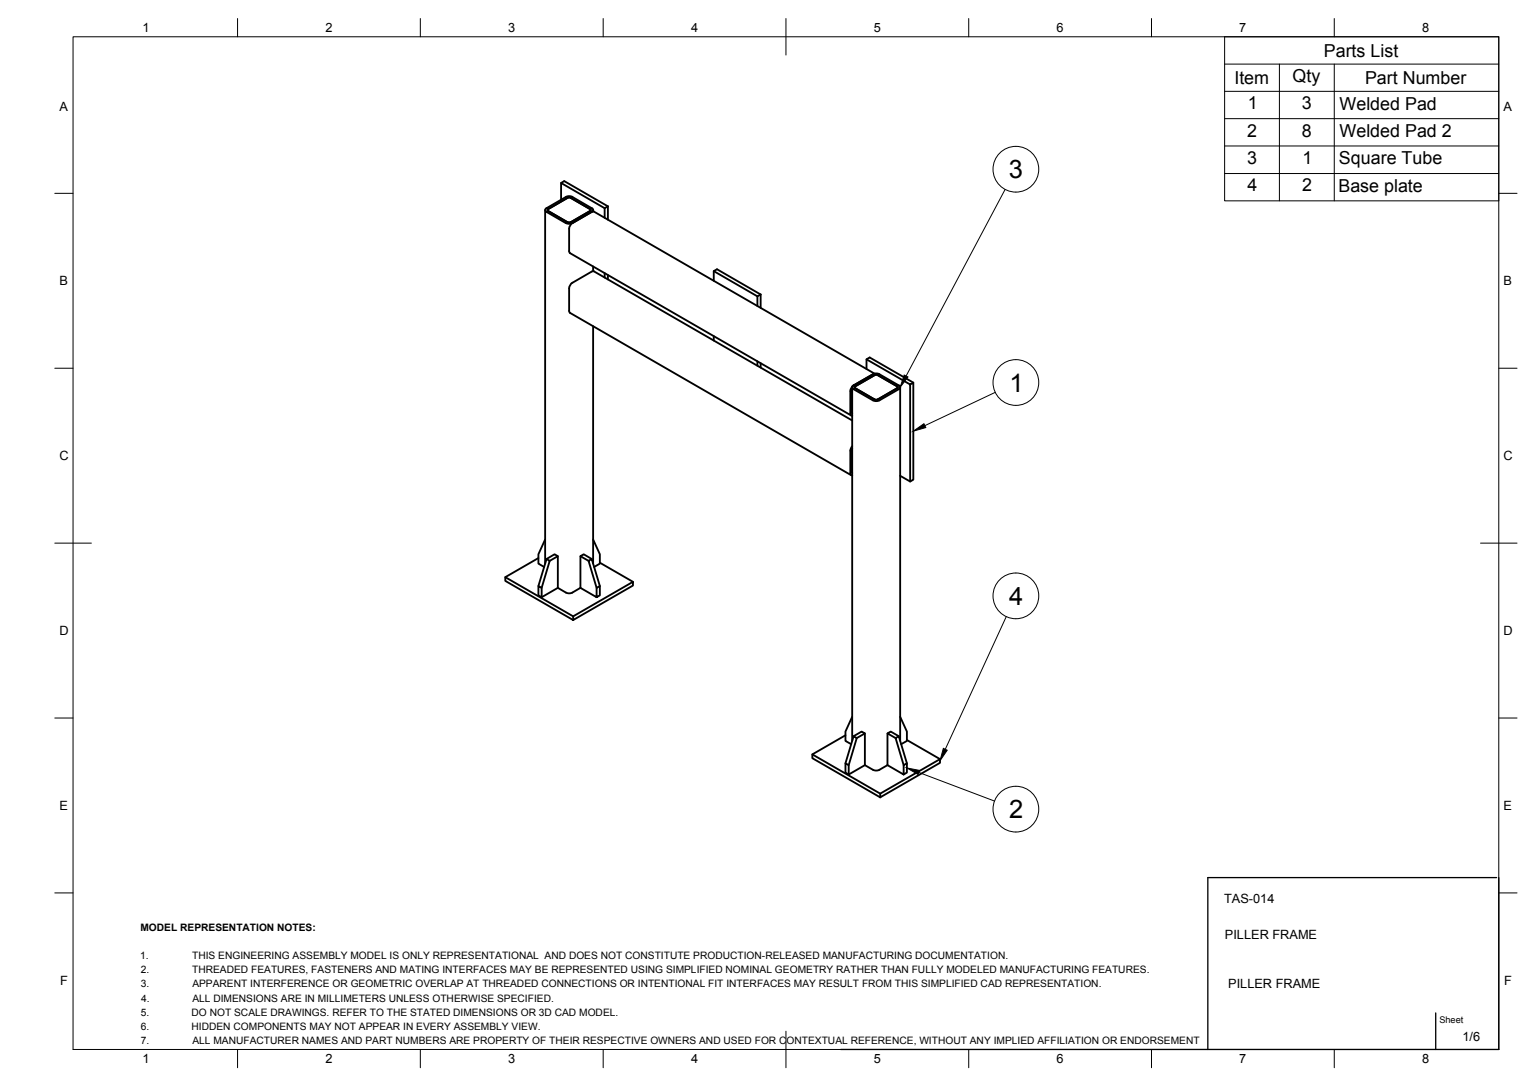
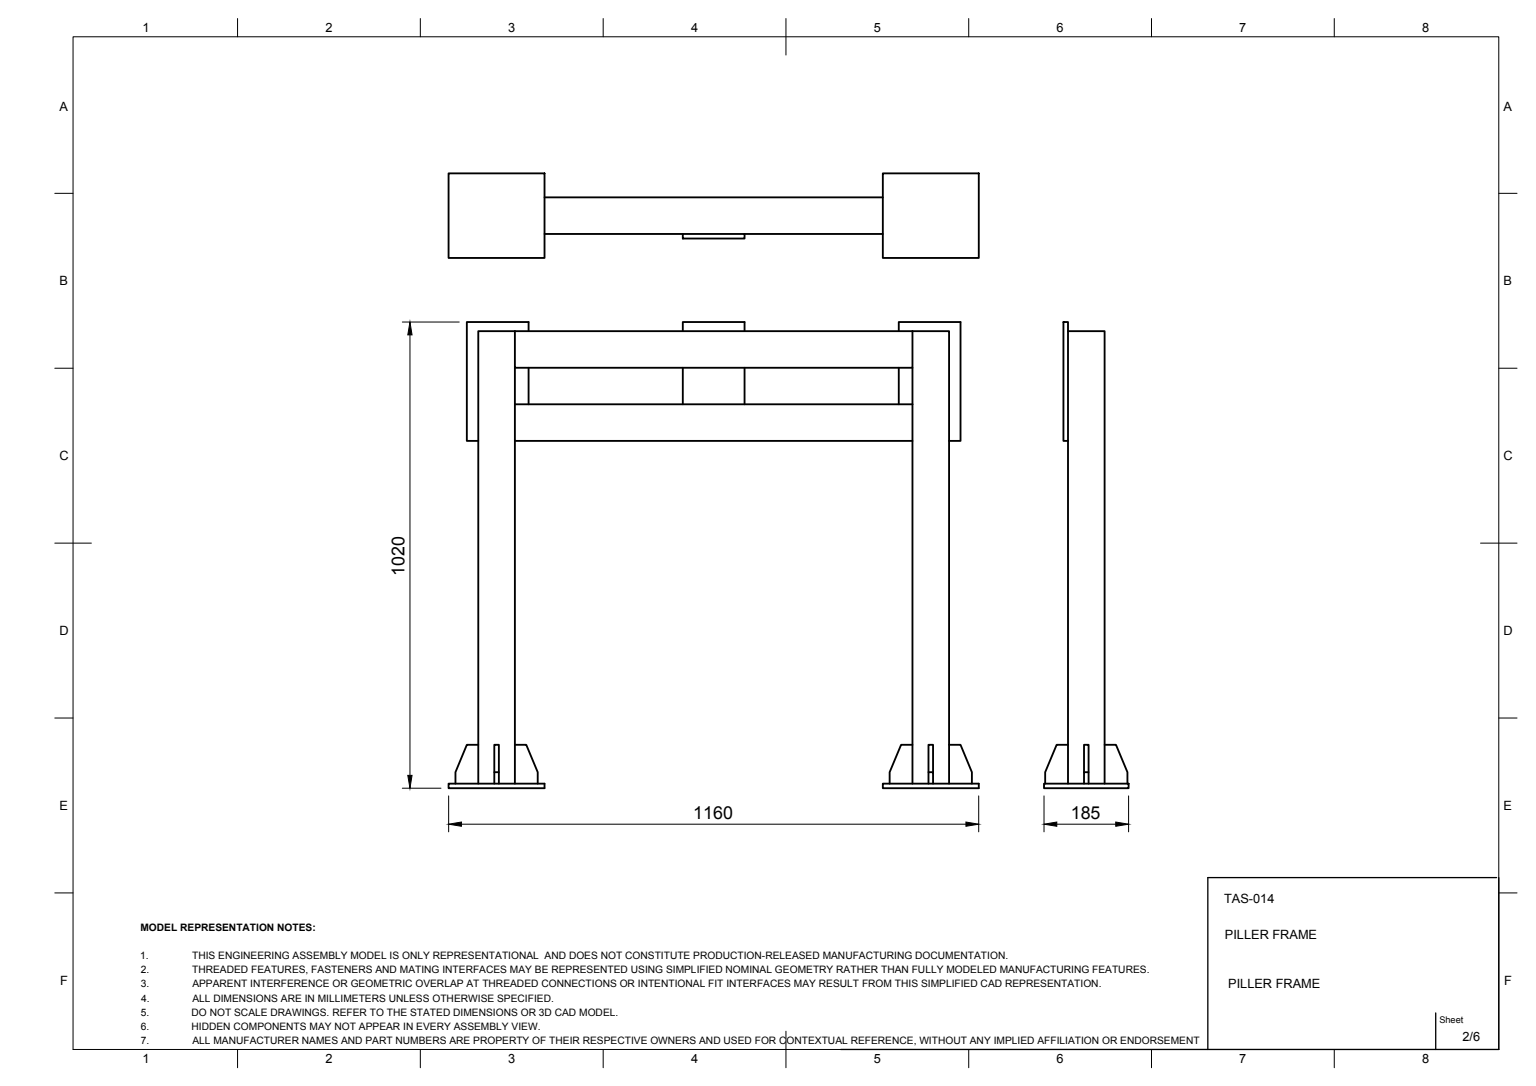
ISO-10303-21;
HEADER;
/* Generated by software containing ST-Developer
 * from STEP Tools, Inc. (www.steptools.com) 
 */

FILE_DESCRIPTION(
/* description */ ('STEP AP214'),
/* implementation_level */ '2;1');

FILE_NAME(
/* name */ 'TAS-014.step',
/* time_stamp */ '2026-11-15T15:22:30-08:00',
/* author */ (''),
/* organization */ (''),
/* preprocessor_version */ 'ST-DEVELOPER v20.2',
/* originating_system */ 'Autodesk Translation Framework v15.17.0.0',
/* authorisation */ '');

FILE_SCHEMA (('AUTOMOTIVE_DESIGN { 1 0 10303 214 3 1 1 }'));
ENDSEC;

DATA;
#10=MECHANICAL_DESIGN_GEOMETRIC_PRESENTATION_REPRESENTATION('',(#79,#80,
#81,#82,#83,#84,#85,#86,#87),#3119);
#11=ITEM_DEFINED_TRANSFORMATION($,$,#2000,#2022);
#12=ITEM_DEFINED_TRANSFORMATION($,$,#2014,#2023);
#13=ITEM_DEFINED_TRANSFORMATION($,$,#1853,#2024);
#14=ITEM_DEFINED_TRANSFORMATION($,$,#2007,#2025);
#15=ITEM_DEFINED_TRANSFORMATION($,$,#2000,#2026);
#16=ITEM_DEFINED_TRANSFORMATION($,$,#2014,#2027);
#17=ITEM_DEFINED_TRANSFORMATION($,$,#2014,#2028);
#18=ITEM_DEFINED_TRANSFORMATION($,$,#2014,#2029);
#19=ITEM_DEFINED_TRANSFORMATION($,$,#2000,#2030);
#20=ITEM_DEFINED_TRANSFORMATION($,$,#2007,#2031);
#21=ITEM_DEFINED_TRANSFORMATION($,$,#2014,#2032);
#22=ITEM_DEFINED_TRANSFORMATION($,$,#2014,#2033);
#23=ITEM_DEFINED_TRANSFORMATION($,$,#2014,#2034);
#24=ITEM_DEFINED_TRANSFORMATION($,$,#2014,#2035);
#25=(
REPRESENTATION_RELATIONSHIP($,$,#3150,#3148)
REPRESENTATION_RELATIONSHIP_WITH_TRANSFORMATION(#11)
SHAPE_REPRESENTATION_RELATIONSHIP()
);
#26=(
REPRESENTATION_RELATIONSHIP($,$,#3152,#3148)
REPRESENTATION_RELATIONSHIP_WITH_TRANSFORMATION(#12)
SHAPE_REPRESENTATION_RELATIONSHIP()
);
#27=(
REPRESENTATION_RELATIONSHIP($,$,#3149,#3148)
REPRESENTATION_RELATIONSHIP_WITH_TRANSFORMATION(#13)
SHAPE_REPRESENTATION_RELATIONSHIP()
);
#28=(
REPRESENTATION_RELATIONSHIP($,$,#3151,#3148)
REPRESENTATION_RELATIONSHIP_WITH_TRANSFORMATION(#14)
SHAPE_REPRESENTATION_RELATIONSHIP()
);
#29=(
REPRESENTATION_RELATIONSHIP($,$,#3150,#3148)
REPRESENTATION_RELATIONSHIP_WITH_TRANSFORMATION(#15)
SHAPE_REPRESENTATION_RELATIONSHIP()
);
#30=(
REPRESENTATION_RELATIONSHIP($,$,#3152,#3148)
REPRESENTATION_RELATIONSHIP_WITH_TRANSFORMATION(#16)
SHAPE_REPRESENTATION_RELATIONSHIP()
);
#31=(
REPRESENTATION_RELATIONSHIP($,$,#3152,#3148)
REPRESENTATION_RELATIONSHIP_WITH_TRANSFORMATION(#17)
SHAPE_REPRESENTATION_RELATIONSHIP()
);
#32=(
REPRESENTATION_RELATIONSHIP($,$,#3152,#3148)
REPRESENTATION_RELATIONSHIP_WITH_TRANSFORMATION(#18)
SHAPE_REPRESENTATION_RELATIONSHIP()
);
#33=(
REPRESENTATION_RELATIONSHIP($,$,#3150,#3148)
REPRESENTATION_RELATIONSHIP_WITH_TRANSFORMATION(#19)
SHAPE_REPRESENTATION_RELATIONSHIP()
);
#34=(
REPRESENTATION_RELATIONSHIP($,$,#3151,#3148)
REPRESENTATION_RELATIONSHIP_WITH_TRANSFORMATION(#20)
SHAPE_REPRESENTATION_RELATIONSHIP()
);
#35=(
REPRESENTATION_RELATIONSHIP($,$,#3152,#3148)
REPRESENTATION_RELATIONSHIP_WITH_TRANSFORMATION(#21)
SHAPE_REPRESENTATION_RELATIONSHIP()
);
#36=(
REPRESENTATION_RELATIONSHIP($,$,#3152,#3148)
REPRESENTATION_RELATIONSHIP_WITH_TRANSFORMATION(#22)
SHAPE_REPRESENTATION_RELATIONSHIP()
);
#37=(
REPRESENTATION_RELATIONSHIP($,$,#3152,#3148)
REPRESENTATION_RELATIONSHIP_WITH_TRANSFORMATION(#23)
SHAPE_REPRESENTATION_RELATIONSHIP()
);
#38=(
REPRESENTATION_RELATIONSHIP($,$,#3152,#3148)
REPRESENTATION_RELATIONSHIP_WITH_TRANSFORMATION(#24)
SHAPE_REPRESENTATION_RELATIONSHIP()
);
#39=CONTEXT_DEPENDENT_SHAPE_REPRESENTATION(#25,#3134);
#40=CONTEXT_DEPENDENT_SHAPE_REPRESENTATION(#26,#3135);
#41=CONTEXT_DEPENDENT_SHAPE_REPRESENTATION(#27,#3136);
#42=CONTEXT_DEPENDENT_SHAPE_REPRESENTATION(#28,#3137);
#43=CONTEXT_DEPENDENT_SHAPE_REPRESENTATION(#29,#3138);
#44=CONTEXT_DEPENDENT_SHAPE_REPRESENTATION(#30,#3139);
#45=CONTEXT_DEPENDENT_SHAPE_REPRESENTATION(#31,#3140);
#46=CONTEXT_DEPENDENT_SHAPE_REPRESENTATION(#32,#3141);
#47=CONTEXT_DEPENDENT_SHAPE_REPRESENTATION(#33,#3142);
#48=CONTEXT_DEPENDENT_SHAPE_REPRESENTATION(#34,#3143);
#49=CONTEXT_DEPENDENT_SHAPE_REPRESENTATION(#35,#3144);
#50=CONTEXT_DEPENDENT_SHAPE_REPRESENTATION(#36,#3145);
#51=CONTEXT_DEPENDENT_SHAPE_REPRESENTATION(#37,#3146);
#52=CONTEXT_DEPENDENT_SHAPE_REPRESENTATION(#38,#3147);
#53=NEXT_ASSEMBLY_USAGE_OCCURRENCE('Welded Pad:1','Welded Pad:1',
'Welded Pad:1',#3154,#3156,'Welded Pad:1');
#54=NEXT_ASSEMBLY_USAGE_OCCURRENCE('Welded Pad 2:1','Welded Pad 2:1',
'Welded Pad 2:1',#3154,#3158,'Welded Pad 2:1');
#55=NEXT_ASSEMBLY_USAGE_OCCURRENCE('Square Tube:1','Square Tube:1',
'Square Tube:1',#3154,#3155,'Square Tube:1');
#56=NEXT_ASSEMBLY_USAGE_OCCURRENCE('Base Plate:1','Base Plate:1',
'Base Plate:1',#3154,#3157,'Base Plate:1');
#57=NEXT_ASSEMBLY_USAGE_OCCURRENCE('Welded Pad:2','Welded Pad:2',
'Welded Pad:2',#3154,#3156,'Welded Pad:2');
#58=NEXT_ASSEMBLY_USAGE_OCCURRENCE('Welded Pad 2:2','Welded Pad 2:2',
'Welded Pad 2:2',#3154,#3158,'Welded Pad 2:2');
#59=NEXT_ASSEMBLY_USAGE_OCCURRENCE('Welded Pad 2:3','Welded Pad 2:3',
'Welded Pad 2:3',#3154,#3158,'Welded Pad 2:3');
#60=NEXT_ASSEMBLY_USAGE_OCCURRENCE('Welded Pad 2:4','Welded Pad 2:4',
'Welded Pad 2:4',#3154,#3158,'Welded Pad 2:4');
#61=NEXT_ASSEMBLY_USAGE_OCCURRENCE('Welded Pad:3','Welded Pad:3',
'Welded Pad:3',#3154,#3156,'Welded Pad:3');
#62=NEXT_ASSEMBLY_USAGE_OCCURRENCE('Base Plate:2','Base Plate:2',
'Base Plate:2',#3154,#3157,'Base Plate:2');
#63=NEXT_ASSEMBLY_USAGE_OCCURRENCE('Welded Pad 2:5','Welded Pad 2:5',
'Welded Pad 2:5',#3154,#3158,'Welded Pad 2:5');
#64=NEXT_ASSEMBLY_USAGE_OCCURRENCE('Welded Pad 2:6','Welded Pad 2:6',
'Welded Pad 2:6',#3154,#3158,'Welded Pad 2:6');
#65=NEXT_ASSEMBLY_USAGE_OCCURRENCE('Welded Pad 2:7','Welded Pad 2:7',
'Welded Pad 2:7',#3154,#3158,'Welded Pad 2:7');
#66=NEXT_ASSEMBLY_USAGE_OCCURRENCE('Welded Pad 2:8','Welded Pad 2:8',
'Welded Pad 2:8',#3154,#3158,'Welded Pad 2:8');
#67=SHAPE_REPRESENTATION_RELATIONSHIP('SRR','None',#3149,#71);
#68=SHAPE_REPRESENTATION_RELATIONSHIP('SRR','None',#3150,#72);
#69=SHAPE_REPRESENTATION_RELATIONSHIP('SRR','None',#3151,#73);
#70=SHAPE_REPRESENTATION_RELATIONSHIP('SRR','None',#3152,#74);
#71=ADVANCED_BREP_SHAPE_REPRESENTATION('',(#88,#89,#90,#91),#3115);
#72=ADVANCED_BREP_SHAPE_REPRESENTATION('',(#92),#3116);
#73=ADVANCED_BREP_SHAPE_REPRESENTATION('',(#93),#3117);
#74=ADVANCED_BREP_SHAPE_REPRESENTATION('',(#94),#3118);
#75=OPEN_SHELL('',(#1779));
#76=OPEN_SHELL('',(#1780));
#77=SHELL_BASED_SURFACE_MODEL('Body5',(#75));
#78=SHELL_BASED_SURFACE_MODEL('Body6',(#76));
#79=STYLED_ITEM('',(#3178),#88);
#80=STYLED_ITEM('',(#3178),#89);
#81=STYLED_ITEM('',(#3178),#90);
#82=STYLED_ITEM('',(#3178),#91);
#83=STYLED_ITEM('',(#3178),#77);
#84=STYLED_ITEM('',(#3178),#78);
#85=STYLED_ITEM('',(#3178),#92);
#86=STYLED_ITEM('',(#3178),#93);
#87=STYLED_ITEM('',(#3178),#94);
#88=MANIFOLD_SOLID_BREP('Body1',#1800);
#89=MANIFOLD_SOLID_BREP('Body2',#1801);
#90=MANIFOLD_SOLID_BREP('Body3',#1802);
#91=MANIFOLD_SOLID_BREP('Body4',#1803);
#92=MANIFOLD_SOLID_BREP('Body1',#1804);
#93=MANIFOLD_SOLID_BREP('Body1',#1805);
#94=MANIFOLD_SOLID_BREP('Body1',#1806);
#95=FACE_BOUND('',#317,.T.);
#96=FACE_BOUND('',#319,.T.);
#97=FACE_BOUND('',#337,.T.);
#98=FACE_BOUND('',#339,.T.);
#99=FACE_BOUND('',#357,.T.);
#100=FACE_BOUND('',#359,.T.);
#101=FACE_BOUND('',#377,.T.);
#102=FACE_BOUND('',#379,.T.);
#103=CIRCLE('',#1856,5.);
#104=CIRCLE('',#1857,5.);
#105=CIRCLE('',#1860,5.);
#106=CIRCLE('',#1861,5.);
#107=CIRCLE('',#1864,5.);
#108=CIRCLE('',#1865,5.);
#109=CIRCLE('',#1868,5.);
#110=CIRCLE('',#1869,5.);
#111=CIRCLE('',#1872,10.);
#112=CIRCLE('',#1873,10.);
#113=CIRCLE('',#1876,10.);
#114=CIRCLE('',#1877,10.);
#115=CIRCLE('',#1880,10.);
#116=CIRCLE('',#1881,10.);
#117=CIRCLE('',#1884,10.);
#118=CIRCLE('',#1885,10.);
#119=CIRCLE('',#1890,5.);
#120=CIRCLE('',#1891,5.);
#121=CIRCLE('',#1894,5.);
#122=CIRCLE('',#1895,5.);
#123=CIRCLE('',#1898,5.);
#124=CIRCLE('',#1899,5.);
#125=CIRCLE('',#1902,5.);
#126=CIRCLE('',#1903,5.);
#127=CIRCLE('',#1906,10.);
#128=CIRCLE('',#1907,10.);
#129=CIRCLE('',#1910,10.);
#130=CIRCLE('',#1911,10.);
#131=CIRCLE('',#1914,10.);
#132=CIRCLE('',#1915,10.);
#133=CIRCLE('',#1918,10.);
#134=CIRCLE('',#1919,10.);
#135=CIRCLE('',#1923,10.);
#136=CIRCLE('',#1924,10.);
#137=CIRCLE('',#1927,10.);
#138=CIRCLE('',#1928,10.);
#139=CIRCLE('',#1931,10.);
#140=CIRCLE('',#1932,10.);
#141=CIRCLE('',#1935,10.);
#142=CIRCLE('',#1936,10.);
#143=CIRCLE('',#1938,5.);
#144=CIRCLE('',#1939,5.);
#145=CIRCLE('',#1942,5.);
#146=CIRCLE('',#1943,5.);
#147=CIRCLE('',#1946,5.);
#148=CIRCLE('',#1947,5.);
#149=CIRCLE('',#1950,5.);
#150=CIRCLE('',#1951,5.);
#151=CIRCLE('',#1957,10.);
#152=CIRCLE('',#1958,10.);
#153=CIRCLE('',#1961,10.);
#154=CIRCLE('',#1962,10.);
#155=CIRCLE('',#1965,10.);
#156=CIRCLE('',#1966,10.);
#157=CIRCLE('',#1969,10.);
#158=CIRCLE('',#1970,10.);
#159=CIRCLE('',#1972,5.);
#160=CIRCLE('',#1973,5.);
#161=CIRCLE('',#1976,5.);
#162=CIRCLE('',#1977,5.);
#163=CIRCLE('',#1980,5.);
#164=CIRCLE('',#1981,5.);
#165=CIRCLE('',#1984,5.);
#166=CIRCLE('',#1985,5.);
#167=CIRCLE('',#1991,5.);
#168=CIRCLE('',#1992,5.);
#169=CIRCLE('',#1993,5.);
#170=CIRCLE('',#1994,5.);
#171=CIRCLE('',#1996,5.);
#172=CIRCLE('',#1997,5.);
#173=CIRCLE('',#1998,5.);
#174=CIRCLE('',#1999,5.);
#175=CYLINDRICAL_SURFACE('',#1855,5.);
#176=CYLINDRICAL_SURFACE('',#1859,5.);
#177=CYLINDRICAL_SURFACE('',#1863,5.);
#178=CYLINDRICAL_SURFACE('',#1867,5.);
#179=CYLINDRICAL_SURFACE('',#1871,10.);
#180=CYLINDRICAL_SURFACE('',#1875,10.);
#181=CYLINDRICAL_SURFACE('',#1879,10.);
#182=CYLINDRICAL_SURFACE('',#1883,10.);
#183=CYLINDRICAL_SURFACE('',#1889,5.);
#184=CYLINDRICAL_SURFACE('',#1893,5.);
#185=CYLINDRICAL_SURFACE('',#1897,5.);
#186=CYLINDRICAL_SURFACE('',#1901,5.);
#187=CYLINDRICAL_SURFACE('',#1905,10.);
#188=CYLINDRICAL_SURFACE('',#1909,10.);
#189=CYLINDRICAL_SURFACE('',#1913,10.);
#190=CYLINDRICAL_SURFACE('',#1917,10.);
#191=CYLINDRICAL_SURFACE('',#1922,10.);
#192=CYLINDRICAL_SURFACE('',#1926,10.);
#193=CYLINDRICAL_SURFACE('',#1930,10.);
#194=CYLINDRICAL_SURFACE('',#1934,10.);
#195=CYLINDRICAL_SURFACE('',#1937,5.);
#196=CYLINDRICAL_SURFACE('',#1941,5.);
#197=CYLINDRICAL_SURFACE('',#1945,5.);
#198=CYLINDRICAL_SURFACE('',#1949,5.);
#199=CYLINDRICAL_SURFACE('',#1956,10.);
#200=CYLINDRICAL_SURFACE('',#1960,10.);
#201=CYLINDRICAL_SURFACE('',#1964,10.);
#202=CYLINDRICAL_SURFACE('',#1968,10.);
#203=CYLINDRICAL_SURFACE('',#1971,5.);
#204=CYLINDRICAL_SURFACE('',#1975,5.);
#205=CYLINDRICAL_SURFACE('',#1979,5.);
#206=CYLINDRICAL_SURFACE('',#1983,5.);
#207=FACE_OUTER_BOUND('',#300,.T.);
#208=FACE_OUTER_BOUND('',#301,.T.);
#209=FACE_OUTER_BOUND('',#302,.T.);
#210=FACE_OUTER_BOUND('',#303,.T.);
#211=FACE_OUTER_BOUND('',#304,.T.);
#212=FACE_OUTER_BOUND('',#305,.T.);
#213=FACE_OUTER_BOUND('',#306,.T.);
#214=FACE_OUTER_BOUND('',#307,.T.);
#215=FACE_OUTER_BOUND('',#308,.T.);
#216=FACE_OUTER_BOUND('',#309,.T.);
#217=FACE_OUTER_BOUND('',#310,.T.);
#218=FACE_OUTER_BOUND('',#311,.T.);
#219=FACE_OUTER_BOUND('',#312,.T.);
#220=FACE_OUTER_BOUND('',#313,.T.);
#221=FACE_OUTER_BOUND('',#314,.T.);
#222=FACE_OUTER_BOUND('',#315,.T.);
#223=FACE_OUTER_BOUND('',#316,.T.);
#224=FACE_OUTER_BOUND('',#318,.T.);
#225=FACE_OUTER_BOUND('',#320,.T.);
#226=FACE_OUTER_BOUND('',#321,.T.);
#227=FACE_OUTER_BOUND('',#322,.T.);
#228=FACE_OUTER_BOUND('',#323,.T.);
#229=FACE_OUTER_BOUND('',#324,.T.);
#230=FACE_OUTER_BOUND('',#325,.T.);
#231=FACE_OUTER_BOUND('',#326,.T.);
#232=FACE_OUTER_BOUND('',#327,.T.);
#233=FACE_OUTER_BOUND('',#328,.T.);
#234=FACE_OUTER_BOUND('',#329,.T.);
#235=FACE_OUTER_BOUND('',#330,.T.);
#236=FACE_OUTER_BOUND('',#331,.T.);
#237=FACE_OUTER_BOUND('',#332,.T.);
#238=FACE_OUTER_BOUND('',#333,.T.);
#239=FACE_OUTER_BOUND('',#334,.T.);
#240=FACE_OUTER_BOUND('',#335,.T.);
#241=FACE_OUTER_BOUND('',#336,.T.);
#242=FACE_OUTER_BOUND('',#338,.T.);
#243=FACE_OUTER_BOUND('',#340,.T.);
#244=FACE_OUTER_BOUND('',#341,.T.);
#245=FACE_OUTER_BOUND('',#342,.T.);
#246=FACE_OUTER_BOUND('',#343,.T.);
#247=FACE_OUTER_BOUND('',#344,.T.);
#248=FACE_OUTER_BOUND('',#345,.T.);
#249=FACE_OUTER_BOUND('',#346,.T.);
#250=FACE_OUTER_BOUND('',#347,.T.);
#251=FACE_OUTER_BOUND('',#348,.T.);
#252=FACE_OUTER_BOUND('',#349,.T.);
#253=FACE_OUTER_BOUND('',#350,.T.);
#254=FACE_OUTER_BOUND('',#351,.T.);
#255=FACE_OUTER_BOUND('',#352,.T.);
#256=FACE_OUTER_BOUND('',#353,.T.);
#257=FACE_OUTER_BOUND('',#354,.T.);
#258=FACE_OUTER_BOUND('',#355,.T.);
#259=FACE_OUTER_BOUND('',#356,.T.);
#260=FACE_OUTER_BOUND('',#358,.T.);
#261=FACE_OUTER_BOUND('',#360,.T.);
#262=FACE_OUTER_BOUND('',#361,.T.);
#263=FACE_OUTER_BOUND('',#362,.T.);
#264=FACE_OUTER_BOUND('',#363,.T.);
#265=FACE_OUTER_BOUND('',#364,.T.);
#266=FACE_OUTER_BOUND('',#365,.T.);
#267=FACE_OUTER_BOUND('',#366,.T.);
#268=FACE_OUTER_BOUND('',#367,.T.);
#269=FACE_OUTER_BOUND('',#368,.T.);
#270=FACE_OUTER_BOUND('',#369,.T.);
#271=FACE_OUTER_BOUND('',#370,.T.);
#272=FACE_OUTER_BOUND('',#371,.T.);
#273=FACE_OUTER_BOUND('',#372,.T.);
#274=FACE_OUTER_BOUND('',#373,.T.);
#275=FACE_OUTER_BOUND('',#374,.T.);
#276=FACE_OUTER_BOUND('',#375,.T.);
#277=FACE_OUTER_BOUND('',#376,.T.);
#278=FACE_OUTER_BOUND('',#378,.T.);
#279=FACE_OUTER_BOUND('',#380,.T.);
#280=FACE_OUTER_BOUND('',#381,.T.);
#281=FACE_OUTER_BOUND('',#382,.T.);
#282=FACE_OUTER_BOUND('',#383,.T.);
#283=FACE_OUTER_BOUND('',#384,.T.);
#284=FACE_OUTER_BOUND('',#385,.T.);
#285=FACE_OUTER_BOUND('',#386,.T.);
#286=FACE_OUTER_BOUND('',#387,.T.);
#287=FACE_OUTER_BOUND('',#388,.T.);
#288=FACE_OUTER_BOUND('',#389,.T.);
#289=FACE_OUTER_BOUND('',#390,.T.);
#290=FACE_OUTER_BOUND('',#391,.T.);
#291=FACE_OUTER_BOUND('',#392,.T.);
#292=FACE_OUTER_BOUND('',#393,.T.);
#293=FACE_OUTER_BOUND('',#394,.T.);
#294=FACE_OUTER_BOUND('',#395,.T.);
#295=FACE_OUTER_BOUND('',#396,.T.);
#296=FACE_OUTER_BOUND('',#397,.T.);
#297=FACE_OUTER_BOUND('',#398,.T.);
#298=FACE_OUTER_BOUND('',#399,.T.);
#299=FACE_OUTER_BOUND('',#400,.T.);
#300=EDGE_LOOP('',(#1168,#1169,#1170,#1171));
#301=EDGE_LOOP('',(#1172,#1173,#1174,#1175));
#302=EDGE_LOOP('',(#1176,#1177,#1178,#1179));
#303=EDGE_LOOP('',(#1180,#1181,#1182,#1183));
#304=EDGE_LOOP('',(#1184,#1185,#1186,#1187));
#305=EDGE_LOOP('',(#1188,#1189,#1190,#1191));
#306=EDGE_LOOP('',(#1192,#1193,#1194,#1195));
#307=EDGE_LOOP('',(#1196,#1197,#1198,#1199));
#308=EDGE_LOOP('',(#1200,#1201,#1202,#1203));
#309=EDGE_LOOP('',(#1204,#1205,#1206,#1207));
#310=EDGE_LOOP('',(#1208,#1209,#1210,#1211));
#311=EDGE_LOOP('',(#1212,#1213,#1214,#1215));
#312=EDGE_LOOP('',(#1216,#1217,#1218,#1219));
#313=EDGE_LOOP('',(#1220,#1221,#1222,#1223));
#314=EDGE_LOOP('',(#1224,#1225,#1226,#1227));
#315=EDGE_LOOP('',(#1228,#1229,#1230,#1231));
#316=EDGE_LOOP('',(#1232,#1233,#1234,#1235,#1236,#1237,#1238,#1239));
#317=EDGE_LOOP('',(#1240,#1241,#1242,#1243,#1244,#1245,#1246,#1247));
#318=EDGE_LOOP('',(#1248,#1249,#1250,#1251,#1252,#1253,#1254,#1255));
#319=EDGE_LOOP('',(#1256,#1257,#1258,#1259,#1260,#1261,#1262,#1263));
#320=EDGE_LOOP('',(#1264,#1265,#1266,#1267));
#321=EDGE_LOOP('',(#1268,#1269,#1270,#1271));
#322=EDGE_LOOP('',(#1272,#1273,#1274,#1275));
#323=EDGE_LOOP('',(#1276,#1277,#1278,#1279));
#324=EDGE_LOOP('',(#1280,#1281,#1282,#1283));
#325=EDGE_LOOP('',(#1284,#1285,#1286,#1287));
#326=EDGE_LOOP('',(#1288,#1289,#1290,#1291));
#327=EDGE_LOOP('',(#1292,#1293,#1294,#1295));
#328=EDGE_LOOP('',(#1296,#1297,#1298,#1299));
#329=EDGE_LOOP('',(#1300,#1301,#1302,#1303));
#330=EDGE_LOOP('',(#1304,#1305,#1306,#1307));
#331=EDGE_LOOP('',(#1308,#1309,#1310,#1311));
#332=EDGE_LOOP('',(#1312,#1313,#1314,#1315));
#333=EDGE_LOOP('',(#1316,#1317,#1318,#1319));
#334=EDGE_LOOP('',(#1320,#1321,#1322,#1323));
#335=EDGE_LOOP('',(#1324,#1325,#1326,#1327));
#336=EDGE_LOOP('',(#1328,#1329,#1330,#1331,#1332,#1333,#1334,#1335));
#337=EDGE_LOOP('',(#1336,#1337,#1338,#1339,#1340,#1341,#1342,#1343));
#338=EDGE_LOOP('',(#1344,#1345,#1346,#1347,#1348,#1349,#1350,#1351));
#339=EDGE_LOOP('',(#1352,#1353,#1354,#1355,#1356,#1357,#1358,#1359));
#340=EDGE_LOOP('',(#1360,#1361,#1362,#1363));
#341=EDGE_LOOP('',(#1364,#1365,#1366,#1367));
#342=EDGE_LOOP('',(#1368,#1369,#1370,#1371));
#343=EDGE_LOOP('',(#1372,#1373,#1374,#1375));
#344=EDGE_LOOP('',(#1376,#1377,#1378,#1379));
#345=EDGE_LOOP('',(#1380,#1381,#1382,#1383));
#346=EDGE_LOOP('',(#1384,#1385,#1386,#1387));
#347=EDGE_LOOP('',(#1388,#1389,#1390,#1391));
#348=EDGE_LOOP('',(#1392,#1393,#1394,#1395));
#349=EDGE_LOOP('',(#1396,#1397,#1398,#1399));
#350=EDGE_LOOP('',(#1400,#1401,#1402,#1403));
#351=EDGE_LOOP('',(#1404,#1405,#1406,#1407));
#352=EDGE_LOOP('',(#1408,#1409,#1410,#1411));
#353=EDGE_LOOP('',(#1412,#1413,#1414,#1415));
#354=EDGE_LOOP('',(#1416,#1417,#1418,#1419));
#355=EDGE_LOOP('',(#1420,#1421,#1422,#1423));
#356=EDGE_LOOP('',(#1424,#1425,#1426,#1427,#1428,#1429,#1430,#1431));
#357=EDGE_LOOP('',(#1432,#1433,#1434,#1435,#1436,#1437,#1438,#1439));
#358=EDGE_LOOP('',(#1440,#1441,#1442,#1443,#1444,#1445,#1446,#1447));
#359=EDGE_LOOP('',(#1448,#1449,#1450,#1451,#1452,#1453,#1454,#1455));
#360=EDGE_LOOP('',(#1456,#1457,#1458,#1459));
#361=EDGE_LOOP('',(#1460,#1461,#1462,#1463));
#362=EDGE_LOOP('',(#1464,#1465,#1466,#1467));
#363=EDGE_LOOP('',(#1468,#1469,#1470,#1471));
#364=EDGE_LOOP('',(#1472,#1473,#1474,#1475));
#365=EDGE_LOOP('',(#1476,#1477,#1478,#1479));
#366=EDGE_LOOP('',(#1480,#1481,#1482,#1483));
#367=EDGE_LOOP('',(#1484,#1485,#1486,#1487));
#368=EDGE_LOOP('',(#1488,#1489,#1490,#1491));
#369=EDGE_LOOP('',(#1492,#1493,#1494,#1495));
#370=EDGE_LOOP('',(#1496,#1497,#1498,#1499));
#371=EDGE_LOOP('',(#1500,#1501,#1502,#1503));
#372=EDGE_LOOP('',(#1504,#1505,#1506,#1507));
#373=EDGE_LOOP('',(#1508,#1509,#1510,#1511));
#374=EDGE_LOOP('',(#1512,#1513,#1514,#1515));
#375=EDGE_LOOP('',(#1516,#1517,#1518,#1519));
#376=EDGE_LOOP('',(#1520,#1521,#1522,#1523,#1524,#1525,#1526,#1527));
#377=EDGE_LOOP('',(#1528,#1529,#1530,#1531,#1532,#1533,#1534,#1535));
#378=EDGE_LOOP('',(#1536,#1537,#1538,#1539,#1540,#1541,#1542,#1543));
#379=EDGE_LOOP('',(#1544,#1545,#1546,#1547,#1548,#1549,#1550,#1551));
#380=EDGE_LOOP('',(#1552,#1553,#1554,#1555,#1556,#1557,#1558,#1559));
#381=EDGE_LOOP('',(#1560,#1561,#1562,#1563,#1564,#1565,#1566,#1567));
#382=EDGE_LOOP('',(#1568,#1569,#1570,#1571));
#383=EDGE_LOOP('',(#1572,#1573,#1574,#1575));
#384=EDGE_LOOP('',(#1576,#1577,#1578,#1579));
#385=EDGE_LOOP('',(#1580,#1581,#1582,#1583));
#386=EDGE_LOOP('',(#1584,#1585,#1586,#1587));
#387=EDGE_LOOP('',(#1588,#1589,#1590,#1591));
#388=EDGE_LOOP('',(#1592,#1593,#1594,#1595));
#389=EDGE_LOOP('',(#1596,#1597,#1598,#1599));
#390=EDGE_LOOP('',(#1600,#1601,#1602,#1603));
#391=EDGE_LOOP('',(#1604,#1605,#1606,#1607));
#392=EDGE_LOOP('',(#1608,#1609,#1610,#1611));
#393=EDGE_LOOP('',(#1612,#1613,#1614,#1615));
#394=EDGE_LOOP('',(#1616,#1617,#1618,#1619));
#395=EDGE_LOOP('',(#1620,#1621,#1622,#1623));
#396=EDGE_LOOP('',(#1624,#1625,#1626,#1627));
#397=EDGE_LOOP('',(#1628,#1629,#1630,#1631));
#398=EDGE_LOOP('',(#1632,#1633,#1634,#1635));
#399=EDGE_LOOP('',(#1636,#1637,#1638,#1639,#1640));
#400=EDGE_LOOP('',(#1641,#1642,#1643,#1644,#1645));
#401=LINE('',#2584,#576);
#402=LINE('',#2586,#577);
#403=LINE('',#2588,#578);
#404=LINE('',#2589,#579);
#405=LINE('',#2593,#580);
#406=LINE('',#2599,#581);
#407=LINE('',#2600,#582);
#408=LINE('',#2601,#583);
#409=LINE('',#2605,#584);
#410=LINE('',#2611,#585);
#411=LINE('',#2612,#586);
#412=LINE('',#2613,#587);
#413=LINE('',#2617,#588);
#414=LINE('',#2623,#589);
#415=LINE('',#2624,#590);
#416=LINE('',#2625,#591);
#417=LINE('',#2632,#592);
#418=LINE('',#2634,#593);
#419=LINE('',#2636,#594);
#420=LINE('',#2637,#595);
#421=LINE('',#2643,#596);
#422=LINE('',#2646,#597);
#423=LINE('',#2648,#598);
#424=LINE('',#2649,#599);
#425=LINE('',#2655,#600);
#426=LINE('',#2658,#601);
#427=LINE('',#2660,#602);
#428=LINE('',#2661,#603);
#429=LINE('',#2667,#604);
#430=LINE('',#2670,#605);
#431=LINE('',#2672,#606);
#432=LINE('',#2673,#607);
#433=LINE('',#2682,#608);
#434=LINE('',#2684,#609);
#435=LINE('',#2686,#610);
#436=LINE('',#2687,#611);
#437=LINE('',#2691,#612);
#438=LINE('',#2697,#613);
#439=LINE('',#2698,#614);
#440=LINE('',#2699,#615);
#441=LINE('',#2703,#616);
#442=LINE('',#2709,#617);
#443=LINE('',#2710,#618);
#444=LINE('',#2711,#619);
#445=LINE('',#2715,#620);
#446=LINE('',#2721,#621);
#447=LINE('',#2722,#622);
#448=LINE('',#2723,#623);
#449=LINE('',#2730,#624);
#450=LINE('',#2732,#625);
#451=LINE('',#2734,#626);
#452=LINE('',#2735,#627);
#453=LINE('',#2741,#628);
#454=LINE('',#2744,#629);
#455=LINE('',#2746,#630);
#456=LINE('',#2747,#631);
#457=LINE('',#2753,#632);
#458=LINE('',#2756,#633);
#459=LINE('',#2758,#634);
#460=LINE('',#2759,#635);
#461=LINE('',#2765,#636);
#462=LINE('',#2768,#637);
#463=LINE('',#2770,#638);
#464=LINE('',#2771,#639);
#465=LINE('',#2782,#640);
#466=LINE('',#2785,#641);
#467=LINE('',#2788,#642);
#468=LINE('',#2790,#643);
#469=LINE('',#2791,#644);
#470=LINE('',#2797,#645);
#471=LINE('',#2800,#646);
#472=LINE('',#2802,#647);
#473=LINE('',#2803,#648);
#474=LINE('',#2809,#649);
#475=LINE('',#2812,#650);
#476=LINE('',#2814,#651);
#477=LINE('',#2815,#652);
#478=LINE('',#2821,#653);
#479=LINE('',#2825,#654);
#480=LINE('',#2829,#655);
#481=LINE('',#2834,#656);
#482=LINE('',#2835,#657);
#483=LINE('',#2836,#658);
#484=LINE('',#2840,#659);
#485=LINE('',#2846,#660);
#486=LINE('',#2847,#661);
#487=LINE('',#2848,#662);
#488=LINE('',#2852,#663);
#489=LINE('',#2858,#664);
#490=LINE('',#2859,#665);
#491=LINE('',#2860,#666);
#492=LINE('',#2864,#667);
#493=LINE('',#2868,#668);
#494=LINE('',#2869,#669);
#495=LINE('',#2871,#670);
#496=LINE('',#2872,#671);
#497=LINE('',#2880,#672);
#498=LINE('',#2883,#673);
#499=LINE('',#2886,#674);
#500=LINE('',#2888,#675);
#501=LINE('',#2889,#676);
#502=LINE('',#2895,#677);
#503=LINE('',#2898,#678);
#504=LINE('',#2900,#679);
#505=LINE('',#2901,#680);
#506=LINE('',#2907,#681);
#507=LINE('',#2910,#682);
#508=LINE('',#2912,#683);
#509=LINE('',#2913,#684);
#510=LINE('',#2919,#685);
#511=LINE('',#2923,#686);
#512=LINE('',#2927,#687);
#513=LINE('',#2932,#688);
#514=LINE('',#2933,#689);
#515=LINE('',#2934,#690);
#516=LINE('',#2938,#691);
#517=LINE('',#2944,#692);
#518=LINE('',#2945,#693);
#519=LINE('',#2946,#694);
#520=LINE('',#2950,#695);
#521=LINE('',#2956,#696);
#522=LINE('',#2957,#697);
#523=LINE('',#2958,#698);
#524=LINE('',#2962,#699);
#525=LINE('',#2966,#700);
#526=LINE('',#2967,#701);
#527=LINE('',#2969,#702);
#528=LINE('',#2970,#703);
#529=LINE('',#2978,#704);
#530=LINE('',#2982,#705);
#531=LINE('',#2986,#706);
#532=LINE('',#2989,#707);
#533=LINE('',#2993,#708);
#534=LINE('',#2997,#709);
#535=LINE('',#3001,#710);
#536=LINE('',#3005,#711);
#537=LINE('',#3011,#712);
#538=LINE('',#3013,#713);
#539=LINE('',#3015,#714);
#540=LINE('',#3016,#715);
#541=LINE('',#3019,#716);
#542=LINE('',#3021,#717);
#543=LINE('',#3022,#718);
#544=LINE('',#3025,#719);
#545=LINE('',#3027,#720);
#546=LINE('',#3028,#721);
#547=LINE('',#3030,#722);
#548=LINE('',#3031,#723);
#549=LINE('',#3038,#724);
#550=LINE('',#3040,#725);
#551=LINE('',#3042,#726);
#552=LINE('',#3043,#727);
#553=LINE('',#3046,#728);
#554=LINE('',#3048,#729);
#555=LINE('',#3049,#730);
#556=LINE('',#3052,#731);
#557=LINE('',#3054,#732);
#558=LINE('',#3055,#733);
#559=LINE('',#3057,#734);
#560=LINE('',#3058,#735);
#561=LINE('',#3065,#736);
#562=LINE('',#3067,#737);
#563=LINE('',#3069,#738);
#564=LINE('',#3070,#739);
#565=LINE('',#3073,#740);
#566=LINE('',#3075,#741);
#567=LINE('',#3076,#742);
#568=LINE('',#3079,#743);
#569=LINE('',#3081,#744);
#570=LINE('',#3082,#745);
#571=LINE('',#3085,#746);
#572=LINE('',#3087,#747);
#573=LINE('',#3088,#748);
#574=LINE('',#3090,#749);
#575=LINE('',#3091,#750);
#576=VECTOR('',#2042,1000.);
#577=VECTOR('',#2043,1000.);
#578=VECTOR('',#2044,1000.);
#579=VECTOR('',#2045,1000.);
#580=VECTOR('',#2048,1000.);
#581=VECTOR('',#2055,1000.);
#582=VECTOR('',#2056,1000.);
#583=VECTOR('',#2057,1000.);
#584=VECTOR('',#2060,1000.);
#585=VECTOR('',#2067,1000.);
#586=VECTOR('',#2068,1000.);
#587=VECTOR('',#2069,1000.);
#588=VECTOR('',#2072,1000.);
#589=VECTOR('',#2079,1000.);
#590=VECTOR('',#2080,1000.);
#591=VECTOR('',#2081,1000.);
#592=VECTOR('',#2090,1000.);
#593=VECTOR('',#2091,1000.);
#594=VECTOR('',#2092,1000.);
#595=VECTOR('',#2093,1000.);
#596=VECTOR('',#2100,1000.);
#597=VECTOR('',#2103,1000.);
#598=VECTOR('',#2104,1000.);
#599=VECTOR('',#2105,1000.);
#600=VECTOR('',#2112,1000.);
#601=VECTOR('',#2115,1000.);
#602=VECTOR('',#2116,1000.);
#603=VECTOR('',#2117,1000.);
#604=VECTOR('',#2124,1000.);
#605=VECTOR('',#2127,1000.);
#606=VECTOR('',#2128,1000.);
#607=VECTOR('',#2129,1000.);
#608=VECTOR('',#2142,1000.);
#609=VECTOR('',#2143,1000.);
#610=VECTOR('',#2144,1000.);
#611=VECTOR('',#2145,1000.);
#612=VECTOR('',#2148,1000.);
#613=VECTOR('',#2155,1000.);
#614=VECTOR('',#2156,1000.);
#615=VECTOR('',#2157,1000.);
#616=VECTOR('',#2160,1000.);
#617=VECTOR('',#2167,1000.);
#618=VECTOR('',#2168,1000.);
#619=VECTOR('',#2169,1000.);
#620=VECTOR('',#2172,1000.);
#621=VECTOR('',#2179,1000.);
#622=VECTOR('',#2180,1000.);
#623=VECTOR('',#2181,1000.);
#624=VECTOR('',#2190,1000.);
#625=VECTOR('',#2191,1000.);
#626=VECTOR('',#2192,1000.);
#627=VECTOR('',#2193,1000.);
#628=VECTOR('',#2200,1000.);
#629=VECTOR('',#2203,1000.);
#630=VECTOR('',#2204,1000.);
#631=VECTOR('',#2205,1000.);
#632=VECTOR('',#2212,1000.);
#633=VECTOR('',#2215,1000.);
#634=VECTOR('',#2216,1000.);
#635=VECTOR('',#2217,1000.);
#636=VECTOR('',#2224,1000.);
#637=VECTOR('',#2227,1000.);
#638=VECTOR('',#2228,1000.);
#639=VECTOR('',#2229,1000.);
#640=VECTOR('',#2244,1000.);
#641=VECTOR('',#2247,1000.);
#642=VECTOR('',#2250,1000.);
#643=VECTOR('',#2251,1000.);
#644=VECTOR('',#2252,1000.);
#645=VECTOR('',#2259,1000.);
#646=VECTOR('',#2262,1000.);
#647=VECTOR('',#2263,1000.);
#648=VECTOR('',#2264,1000.);
#649=VECTOR('',#2271,1000.);
#650=VECTOR('',#2274,1000.);
#651=VECTOR('',#2275,1000.);
#652=VECTOR('',#2276,1000.);
#653=VECTOR('',#2283,1000.);
#654=VECTOR('',#2286,1000.);
#655=VECTOR('',#2289,1000.);
#656=VECTOR('',#2294,1000.);
#657=VECTOR('',#2295,1000.);
#658=VECTOR('',#2296,1000.);
#659=VECTOR('',#2299,1000.);
#660=VECTOR('',#2306,1000.);
#661=VECTOR('',#2307,1000.);
#662=VECTOR('',#2308,1000.);
#663=VECTOR('',#2311,1000.);
#664=VECTOR('',#2318,1000.);
#665=VECTOR('',#2319,1000.);
#666=VECTOR('',#2320,1000.);
#667=VECTOR('',#2323,1000.);
#668=VECTOR('',#2330,1000.);
#669=VECTOR('',#2331,1000.);
#670=VECTOR('',#2334,1000.);
#671=VECTOR('',#2335,1000.);
#672=VECTOR('',#2344,1000.);
#673=VECTOR('',#2347,1000.);
#674=VECTOR('',#2350,1000.);
#675=VECTOR('',#2351,1000.);
#676=VECTOR('',#2352,1000.);
#677=VECTOR('',#2359,1000.);
#678=VECTOR('',#2362,1000.);
#679=VECTOR('',#2363,1000.);
#680=VECTOR('',#2364,1000.);
#681=VECTOR('',#2371,1000.);
#682=VECTOR('',#2374,1000.);
#683=VECTOR('',#2375,1000.);
#684=VECTOR('',#2376,1000.);
#685=VECTOR('',#2383,1000.);
#686=VECTOR('',#2386,1000.);
#687=VECTOR('',#2389,1000.);
#688=VECTOR('',#2394,1000.);
#689=VECTOR('',#2395,1000.);
#690=VECTOR('',#2396,1000.);
#691=VECTOR('',#2399,1000.);
#692=VECTOR('',#2406,1000.);
#693=VECTOR('',#2407,1000.);
#694=VECTOR('',#2408,1000.);
#695=VECTOR('',#2411,1000.);
#696=VECTOR('',#2418,1000.);
#697=VECTOR('',#2419,1000.);
#698=VECTOR('',#2420,1000.);
#699=VECTOR('',#2423,1000.);
#700=VECTOR('',#2430,1000.);
#701=VECTOR('',#2431,1000.);
#702=VECTOR('',#2434,1000.);
#703=VECTOR('',#2435,1000.);
#704=VECTOR('',#2444,1000.);
#705=VECTOR('',#2447,1000.);
#706=VECTOR('',#2450,1000.);
#707=VECTOR('',#2453,1000.);
#708=VECTOR('',#2456,1000.);
#709=VECTOR('',#2459,1000.);
#710=VECTOR('',#2462,1000.);
#711=VECTOR('',#2465,1000.);
#712=VECTOR('',#2472,1000.);
#713=VECTOR('',#2473,1000.);
#714=VECTOR('',#2474,1000.);
#715=VECTOR('',#2475,1000.);
#716=VECTOR('',#2478,1000.);
#717=VECTOR('',#2479,1000.);
#718=VECTOR('',#2480,1000.);
#719=VECTOR('',#2483,1000.);
#720=VECTOR('',#2484,1000.);
#721=VECTOR('',#2485,1000.);
#722=VECTOR('',#2488,1000.);
#723=VECTOR('',#2489,1000.);
#724=VECTOR('',#2498,1000.);
#725=VECTOR('',#2499,1000.);
#726=VECTOR('',#2500,1000.);
#727=VECTOR('',#2501,1000.);
#728=VECTOR('',#2504,1000.);
#729=VECTOR('',#2505,1000.);
#730=VECTOR('',#2506,1000.);
#731=VECTOR('',#2509,1000.);
#732=VECTOR('',#2510,1000.);
#733=VECTOR('',#2511,1000.);
#734=VECTOR('',#2514,1000.);
#735=VECTOR('',#2515,1000.);
#736=VECTOR('',#2524,1000.);
#737=VECTOR('',#2525,1000.);
#738=VECTOR('',#2526,1000.);
#739=VECTOR('',#2527,1000.);
#740=VECTOR('',#2530,1000.);
#741=VECTOR('',#2531,1000.);
#742=VECTOR('',#2532,1000.);
#743=VECTOR('',#2535,1000.);
#744=VECTOR('',#2536,1000.);
#745=VECTOR('',#2537,1000.);
#746=VECTOR('',#2540,1000.);
#747=VECTOR('',#2541,1000.);
#748=VECTOR('',#2542,1000.);
#749=VECTOR('',#2545,1000.);
#750=VECTOR('',#2546,1000.);
#751=VERTEX_POINT('',#2582);
#752=VERTEX_POINT('',#2583);
#753=VERTEX_POINT('',#2585);
#754=VERTEX_POINT('',#2587);
#755=VERTEX_POINT('',#2591);
#756=VERTEX_POINT('',#2592);
#757=VERTEX_POINT('',#2597);
#758=VERTEX_POINT('',#2598);
#759=VERTEX_POINT('',#2603);
#760=VERTEX_POINT('',#2604);
#761=VERTEX_POINT('',#2609);
#762=VERTEX_POINT('',#2610);
#763=VERTEX_POINT('',#2615);
#764=VERTEX_POINT('',#2616);
#765=VERTEX_POINT('',#2621);
#766=VERTEX_POINT('',#2622);
#767=VERTEX_POINT('',#2630);
#768=VERTEX_POINT('',#2631);
#769=VERTEX_POINT('',#2633);
#770=VERTEX_POINT('',#2635);
#771=VERTEX_POINT('',#2639);
#772=VERTEX_POINT('',#2641);
#773=VERTEX_POINT('',#2645);
#774=VERTEX_POINT('',#2647);
#775=VERTEX_POINT('',#2651);
#776=VERTEX_POINT('',#2653);
#777=VERTEX_POINT('',#2657);
#778=VERTEX_POINT('',#2659);
#779=VERTEX_POINT('',#2663);
#780=VERTEX_POINT('',#2665);
#781=VERTEX_POINT('',#2669);
#782=VERTEX_POINT('',#2671);
#783=VERTEX_POINT('',#2680);
#784=VERTEX_POINT('',#2681);
#785=VERTEX_POINT('',#2683);
#786=VERTEX_POINT('',#2685);
#787=VERTEX_POINT('',#2689);
#788=VERTEX_POINT('',#2690);
#789=VERTEX_POINT('',#2695);
#790=VERTEX_POINT('',#2696);
#791=VERTEX_POINT('',#2701);
#792=VERTEX_POINT('',#2702);
#793=VERTEX_POINT('',#2707);
#794=VERTEX_POINT('',#2708);
#795=VERTEX_POINT('',#2713);
#796=VERTEX_POINT('',#2714);
#797=VERTEX_POINT('',#2719);
#798=VERTEX_POINT('',#2720);
#799=VERTEX_POINT('',#2728);
#800=VERTEX_POINT('',#2729);
#801=VERTEX_POINT('',#2731);
#802=VERTEX_POINT('',#2733);
#803=VERTEX_POINT('',#2737);
#804=VERTEX_POINT('',#2739);
#805=VERTEX_POINT('',#2743);
#806=VERTEX_POINT('',#2745);
#807=VERTEX_POINT('',#2749);
#808=VERTEX_POINT('',#2751);
#809=VERTEX_POINT('',#2755);
#810=VERTEX_POINT('',#2757);
#811=VERTEX_POINT('',#2761);
#812=VERTEX_POINT('',#2763);
#813=VERTEX_POINT('',#2767);
#814=VERTEX_POINT('',#2769);
#815=VERTEX_POINT('',#2778);
#816=VERTEX_POINT('',#2779);
#817=VERTEX_POINT('',#2781);
#818=VERTEX_POINT('',#2783);
#819=VERTEX_POINT('',#2787);
#820=VERTEX_POINT('',#2789);
#821=VERTEX_POINT('',#2793);
#822=VERTEX_POINT('',#2795);
#823=VERTEX_POINT('',#2799);
#824=VERTEX_POINT('',#2801);
#825=VERTEX_POINT('',#2805);
#826=VERTEX_POINT('',#2807);
#827=VERTEX_POINT('',#2811);
#828=VERTEX_POINT('',#2813);
#829=VERTEX_POINT('',#2817);
#830=VERTEX_POINT('',#2819);
#831=VERTEX_POINT('',#2823);
#832=VERTEX_POINT('',#2824);
#833=VERTEX_POINT('',#2826);
#834=VERTEX_POINT('',#2828);
#835=VERTEX_POINT('',#2832);
#836=VERTEX_POINT('',#2833);
#837=VERTEX_POINT('',#2838);
#838=VERTEX_POINT('',#2839);
#839=VERTEX_POINT('',#2844);
#840=VERTEX_POINT('',#2845);
#841=VERTEX_POINT('',#2850);
#842=VERTEX_POINT('',#2851);
#843=VERTEX_POINT('',#2856);
#844=VERTEX_POINT('',#2857);
#845=VERTEX_POINT('',#2862);
#846=VERTEX_POINT('',#2863);
#847=VERTEX_POINT('',#2876);
#848=VERTEX_POINT('',#2877);
#849=VERTEX_POINT('',#2879);
#850=VERTEX_POINT('',#2881);
#851=VERTEX_POINT('',#2885);
#852=VERTEX_POINT('',#2887);
#853=VERTEX_POINT('',#2891);
#854=VERTEX_POINT('',#2893);
#855=VERTEX_POINT('',#2897);
#856=VERTEX_POINT('',#2899);
#857=VERTEX_POINT('',#2903);
#858=VERTEX_POINT('',#2905);
#859=VERTEX_POINT('',#2909);
#860=VERTEX_POINT('',#2911);
#861=VERTEX_POINT('',#2915);
#862=VERTEX_POINT('',#2917);
#863=VERTEX_POINT('',#2921);
#864=VERTEX_POINT('',#2922);
#865=VERTEX_POINT('',#2924);
#866=VERTEX_POINT('',#2926);
#867=VERTEX_POINT('',#2930);
#868=VERTEX_POINT('',#2931);
#869=VERTEX_POINT('',#2936);
#870=VERTEX_POINT('',#2937);
#871=VERTEX_POINT('',#2942);
#872=VERTEX_POINT('',#2943);
#873=VERTEX_POINT('',#2948);
#874=VERTEX_POINT('',#2949);
#875=VERTEX_POINT('',#2954);
#876=VERTEX_POINT('',#2955);
#877=VERTEX_POINT('',#2960);
#878=VERTEX_POINT('',#2961);
#879=VERTEX_POINT('',#2974);
#880=VERTEX_POINT('',#2975);
#881=VERTEX_POINT('',#2977);
#882=VERTEX_POINT('',#2979);
#883=VERTEX_POINT('',#2981);
#884=VERTEX_POINT('',#2983);
#885=VERTEX_POINT('',#2985);
#886=VERTEX_POINT('',#2987);
#887=VERTEX_POINT('',#2991);
#888=VERTEX_POINT('',#2992);
#889=VERTEX_POINT('',#2994);
#890=VERTEX_POINT('',#2996);
#891=VERTEX_POINT('',#2998);
#892=VERTEX_POINT('',#3000);
#893=VERTEX_POINT('',#3002);
#894=VERTEX_POINT('',#3004);
#895=VERTEX_POINT('',#3009);
#896=VERTEX_POINT('',#3010);
#897=VERTEX_POINT('',#3012);
#898=VERTEX_POINT('',#3014);
#899=VERTEX_POINT('',#3018);
#900=VERTEX_POINT('',#3020);
#901=VERTEX_POINT('',#3024);
#902=VERTEX_POINT('',#3026);
#903=VERTEX_POINT('',#3036);
#904=VERTEX_POINT('',#3037);
#905=VERTEX_POINT('',#3039);
#906=VERTEX_POINT('',#3041);
#907=VERTEX_POINT('',#3045);
#908=VERTEX_POINT('',#3047);
#909=VERTEX_POINT('',#3051);
#910=VERTEX_POINT('',#3053);
#911=VERTEX_POINT('',#3063);
#912=VERTEX_POINT('',#3064);
#913=VERTEX_POINT('',#3066);
#914=VERTEX_POINT('',#3068);
#915=VERTEX_POINT('',#3072);
#916=VERTEX_POINT('',#3074);
#917=VERTEX_POINT('',#3078);
#918=VERTEX_POINT('',#3080);
#919=VERTEX_POINT('',#3084);
#920=VERTEX_POINT('',#3086);
#921=EDGE_CURVE('',#751,#752,#401,.T.);
#922=EDGE_CURVE('',#752,#753,#402,.T.);
#923=EDGE_CURVE('',#754,#753,#403,.T.);
#924=EDGE_CURVE('',#754,#751,#404,.T.);
#925=EDGE_CURVE('',#755,#756,#405,.T.);
#926=EDGE_CURVE('',#756,#752,#103,.T.);
#927=EDGE_CURVE('',#751,#755,#104,.T.);
#928=EDGE_CURVE('',#757,#758,#406,.T.);
#929=EDGE_CURVE('',#758,#756,#407,.T.);
#930=EDGE_CURVE('',#755,#757,#408,.T.);
#931=EDGE_CURVE('',#759,#760,#409,.T.);
#932=EDGE_CURVE('',#760,#758,#105,.T.);
#933=EDGE_CURVE('',#757,#759,#106,.T.);
#934=EDGE_CURVE('',#761,#762,#410,.T.);
#935=EDGE_CURVE('',#762,#760,#411,.T.);
#936=EDGE_CURVE('',#759,#761,#412,.T.);
#937=EDGE_CURVE('',#763,#764,#413,.T.);
#938=EDGE_CURVE('',#764,#762,#107,.T.);
#939=EDGE_CURVE('',#761,#763,#108,.T.);
#940=EDGE_CURVE('',#765,#766,#414,.T.);
#941=EDGE_CURVE('',#766,#764,#415,.T.);
#942=EDGE_CURVE('',#763,#765,#416,.T.);
#943=EDGE_CURVE('',#753,#766,#109,.T.);
#944=EDGE_CURVE('',#765,#754,#110,.T.);
#945=EDGE_CURVE('',#767,#768,#417,.T.);
#946=EDGE_CURVE('',#769,#767,#418,.T.);
#947=EDGE_CURVE('',#770,#769,#419,.T.);
#948=EDGE_CURVE('',#770,#768,#420,.T.);
#949=EDGE_CURVE('',#768,#771,#111,.T.);
#950=EDGE_CURVE('',#772,#770,#112,.T.);
#951=EDGE_CURVE('',#772,#771,#421,.T.);
#952=EDGE_CURVE('',#771,#773,#422,.T.);
#953=EDGE_CURVE('',#772,#774,#423,.T.);
#954=EDGE_CURVE('',#774,#773,#424,.T.);
#955=EDGE_CURVE('',#773,#775,#113,.T.);
#956=EDGE_CURVE('',#776,#774,#114,.T.);
#957=EDGE_CURVE('',#776,#775,#425,.T.);
#958=EDGE_CURVE('',#775,#777,#426,.T.);
#959=EDGE_CURVE('',#778,#776,#427,.T.);
#960=EDGE_CURVE('',#778,#777,#428,.T.);
#961=EDGE_CURVE('',#777,#779,#115,.T.);
#962=EDGE_CURVE('',#780,#778,#116,.T.);
#963=EDGE_CURVE('',#780,#779,#429,.T.);
#964=EDGE_CURVE('',#781,#779,#430,.T.);
#965=EDGE_CURVE('',#782,#780,#431,.T.);
#966=EDGE_CURVE('',#782,#781,#432,.T.);
#967=EDGE_CURVE('',#781,#767,#117,.T.);
#968=EDGE_CURVE('',#769,#782,#118,.T.);
#969=EDGE_CURVE('',#783,#784,#433,.T.);
#970=EDGE_CURVE('',#784,#785,#434,.T.);
#971=EDGE_CURVE('',#786,#785,#435,.T.);
#972=EDGE_CURVE('',#786,#783,#436,.T.);
#973=EDGE_CURVE('',#787,#788,#437,.T.);
#974=EDGE_CURVE('',#788,#784,#119,.T.);
#975=EDGE_CURVE('',#783,#787,#120,.T.);
#976=EDGE_CURVE('',#789,#790,#438,.T.);
#977=EDGE_CURVE('',#790,#788,#439,.T.);
#978=EDGE_CURVE('',#787,#789,#440,.T.);
#979=EDGE_CURVE('',#791,#792,#441,.T.);
#980=EDGE_CURVE('',#792,#790,#121,.T.);
#981=EDGE_CURVE('',#789,#791,#122,.T.);
#982=EDGE_CURVE('',#793,#794,#442,.T.);
#983=EDGE_CURVE('',#794,#792,#443,.T.);
#984=EDGE_CURVE('',#791,#793,#444,.T.);
#985=EDGE_CURVE('',#795,#796,#445,.T.);
#986=EDGE_CURVE('',#796,#794,#123,.T.);
#987=EDGE_CURVE('',#793,#795,#124,.T.);
#988=EDGE_CURVE('',#797,#798,#446,.T.);
#989=EDGE_CURVE('',#798,#796,#447,.T.);
#990=EDGE_CURVE('',#795,#797,#448,.T.);
#991=EDGE_CURVE('',#785,#798,#125,.T.);
#992=EDGE_CURVE('',#797,#786,#126,.T.);
#993=EDGE_CURVE('',#799,#800,#449,.T.);
#994=EDGE_CURVE('',#801,#799,#450,.T.);
#995=EDGE_CURVE('',#802,#801,#451,.T.);
#996=EDGE_CURVE('',#802,#800,#452,.T.);
#997=EDGE_CURVE('',#800,#803,#127,.T.);
#998=EDGE_CURVE('',#804,#802,#128,.T.);
#999=EDGE_CURVE('',#804,#803,#453,.T.);
#1000=EDGE_CURVE('',#803,#805,#454,.T.);
#1001=EDGE_CURVE('',#804,#806,#455,.T.);
#1002=EDGE_CURVE('',#806,#805,#456,.T.);
#1003=EDGE_CURVE('',#805,#807,#129,.T.);
#1004=EDGE_CURVE('',#808,#806,#130,.T.);
#1005=EDGE_CURVE('',#808,#807,#457,.T.);
#1006=EDGE_CURVE('',#807,#809,#458,.T.);
#1007=EDGE_CURVE('',#810,#808,#459,.T.);
#1008=EDGE_CURVE('',#810,#809,#460,.T.);
#1009=EDGE_CURVE('',#809,#811,#131,.T.);
#1010=EDGE_CURVE('',#812,#810,#132,.T.);
#1011=EDGE_CURVE('',#812,#811,#461,.T.);
#1012=EDGE_CURVE('',#813,#811,#462,.T.);
#1013=EDGE_CURVE('',#814,#812,#463,.T.);
#1014=EDGE_CURVE('',#814,#813,#464,.T.);
#1015=EDGE_CURVE('',#813,#799,#133,.T.);
#1016=EDGE_CURVE('',#801,#814,#134,.T.);
#1017=EDGE_CURVE('',#815,#816,#135,.T.);
#1018=EDGE_CURVE('',#815,#817,#465,.T.);
#1019=EDGE_CURVE('',#817,#818,#136,.T.);
#1020=EDGE_CURVE('',#816,#818,#466,.T.);
#1021=EDGE_CURVE('',#816,#819,#467,.T.);
#1022=EDGE_CURVE('',#818,#820,#468,.T.);
#1023=EDGE_CURVE('',#819,#820,#469,.T.);
#1024=EDGE_CURVE('',#819,#821,#137,.T.);
#1025=EDGE_CURVE('',#820,#822,#138,.T.);
#1026=EDGE_CURVE('',#821,#822,#470,.T.);
#1027=EDGE_CURVE('',#821,#823,#471,.T.);
#1028=EDGE_CURVE('',#822,#824,#472,.T.);
#1029=EDGE_CURVE('',#823,#824,#473,.T.);
#1030=EDGE_CURVE('',#823,#825,#139,.T.);
#1031=EDGE_CURVE('',#824,#826,#140,.T.);
#1032=EDGE_CURVE('',#825,#826,#474,.T.);
#1033=EDGE_CURVE('',#825,#827,#475,.T.);
#1034=EDGE_CURVE('',#826,#828,#476,.T.);
#1035=EDGE_CURVE('',#827,#828,#477,.T.);
#1036=EDGE_CURVE('',#827,#829,#141,.T.);
#1037=EDGE_CURVE('',#828,#830,#142,.T.);
#1038=EDGE_CURVE('',#829,#830,#478,.T.);
#1039=EDGE_CURVE('',#831,#832,#479,.T.);
#1040=EDGE_CURVE('',#831,#833,#143,.T.);
#1041=EDGE_CURVE('',#833,#834,#480,.T.);
#1042=EDGE_CURVE('',#832,#834,#144,.T.);
#1043=EDGE_CURVE('',#835,#836,#481,.T.);
#1044=EDGE_CURVE('',#835,#831,#482,.T.);
#1045=EDGE_CURVE('',#836,#832,#483,.T.);
#1046=EDGE_CURVE('',#837,#838,#484,.T.);
#1047=EDGE_CURVE('',#837,#835,#145,.T.);
#1048=EDGE_CURVE('',#838,#836,#146,.T.);
#1049=EDGE_CURVE('',#839,#840,#485,.T.);
#1050=EDGE_CURVE('',#839,#837,#486,.T.);
#1051=EDGE_CURVE('',#840,#838,#487,.T.);
#1052=EDGE_CURVE('',#841,#842,#488,.T.);
#1053=EDGE_CURVE('',#841,#839,#147,.T.);
#1054=EDGE_CURVE('',#842,#840,#148,.T.);
#1055=EDGE_CURVE('',#843,#844,#489,.T.);
#1056=EDGE_CURVE('',#843,#841,#490,.T.);
#1057=EDGE_CURVE('',#844,#842,#491,.T.);
#1058=EDGE_CURVE('',#845,#846,#492,.T.);
#1059=EDGE_CURVE('',#845,#843,#149,.T.);
#1060=EDGE_CURVE('',#846,#844,#150,.T.);
#1061=EDGE_CURVE('',#833,#845,#493,.T.);
#1062=EDGE_CURVE('',#834,#846,#494,.T.);
#1063=EDGE_CURVE('',#829,#815,#495,.T.);
#1064=EDGE_CURVE('',#830,#817,#496,.T.);
#1065=EDGE_CURVE('',#847,#848,#151,.T.);
#1066=EDGE_CURVE('',#847,#849,#497,.T.);
#1067=EDGE_CURVE('',#849,#850,#152,.T.);
#1068=EDGE_CURVE('',#848,#850,#498,.T.);
#1069=EDGE_CURVE('',#848,#851,#499,.T.);
#1070=EDGE_CURVE('',#850,#852,#500,.T.);
#1071=EDGE_CURVE('',#851,#852,#501,.T.);
#1072=EDGE_CURVE('',#851,#853,#153,.T.);
#1073=EDGE_CURVE('',#852,#854,#154,.T.);
#1074=EDGE_CURVE('',#853,#854,#502,.T.);
#1075=EDGE_CURVE('',#853,#855,#503,.T.);
#1076=EDGE_CURVE('',#854,#856,#504,.T.);
#1077=EDGE_CURVE('',#855,#856,#505,.T.);
#1078=EDGE_CURVE('',#855,#857,#155,.T.);
#1079=EDGE_CURVE('',#856,#858,#156,.T.);
#1080=EDGE_CURVE('',#857,#858,#506,.T.);
#1081=EDGE_CURVE('',#857,#859,#507,.T.);
#1082=EDGE_CURVE('',#858,#860,#508,.T.);
#1083=EDGE_CURVE('',#859,#860,#509,.T.);
#1084=EDGE_CURVE('',#859,#861,#157,.T.);
#1085=EDGE_CURVE('',#860,#862,#158,.T.);
#1086=EDGE_CURVE('',#861,#862,#510,.T.);
#1087=EDGE_CURVE('',#863,#864,#511,.T.);
#1088=EDGE_CURVE('',#863,#865,#159,.T.);
#1089=EDGE_CURVE('',#865,#866,#512,.T.);
#1090=EDGE_CURVE('',#864,#866,#160,.T.);
#1091=EDGE_CURVE('',#867,#868,#513,.T.);
#1092=EDGE_CURVE('',#867,#863,#514,.T.);
#1093=EDGE_CURVE('',#868,#864,#515,.T.);
#1094=EDGE_CURVE('',#869,#870,#516,.T.);
#1095=EDGE_CURVE('',#869,#867,#161,.T.);
#1096=EDGE_CURVE('',#870,#868,#162,.T.);
#1097=EDGE_CURVE('',#871,#872,#517,.T.);
#1098=EDGE_CURVE('',#871,#869,#518,.T.);
#1099=EDGE_CURVE('',#872,#870,#519,.T.);
#1100=EDGE_CURVE('',#873,#874,#520,.T.);
#1101=EDGE_CURVE('',#873,#871,#163,.T.);
#1102=EDGE_CURVE('',#874,#872,#164,.T.);
#1103=EDGE_CURVE('',#875,#876,#521,.T.);
#1104=EDGE_CURVE('',#875,#873,#522,.T.);
#1105=EDGE_CURVE('',#876,#874,#523,.T.);
#1106=EDGE_CURVE('',#877,#878,#524,.T.);
#1107=EDGE_CURVE('',#877,#875,#165,.T.);
#1108=EDGE_CURVE('',#878,#876,#166,.T.);
#1109=EDGE_CURVE('',#865,#877,#525,.T.);
#1110=EDGE_CURVE('',#866,#878,#526,.T.);
#1111=EDGE_CURVE('',#861,#847,#527,.T.);
#1112=EDGE_CURVE('',#862,#849,#528,.T.);
#1113=EDGE_CURVE('',#879,#880,#167,.T.);
#1114=EDGE_CURVE('',#880,#881,#529,.T.);
#1115=EDGE_CURVE('',#881,#882,#168,.T.);
#1116=EDGE_CURVE('',#882,#883,#530,.T.);
#1117=EDGE_CURVE('',#883,#884,#169,.T.);
#1118=EDGE_CURVE('',#884,#885,#531,.T.);
#1119=EDGE_CURVE('',#885,#886,#170,.T.);
#1120=EDGE_CURVE('',#886,#879,#532,.T.);
#1121=EDGE_CURVE('',#887,#888,#533,.T.);
#1122=EDGE_CURVE('',#888,#889,#171,.T.);
#1123=EDGE_CURVE('',#889,#890,#534,.T.);
#1124=EDGE_CURVE('',#890,#891,#172,.T.);
#1125=EDGE_CURVE('',#891,#892,#535,.T.);
#1126=EDGE_CURVE('',#892,#893,#173,.T.);
#1127=EDGE_CURVE('',#893,#894,#536,.T.);
#1128=EDGE_CURVE('',#894,#887,#174,.T.);
#1129=EDGE_CURVE('',#895,#896,#537,.T.);
#1130=EDGE_CURVE('',#897,#896,#538,.T.);
#1131=EDGE_CURVE('',#898,#897,#539,.T.);
#1132=EDGE_CURVE('',#898,#895,#540,.T.);
#1133=EDGE_CURVE('',#896,#899,#541,.T.);
#1134=EDGE_CURVE('',#900,#899,#542,.T.);
#1135=EDGE_CURVE('',#897,#900,#543,.T.);
#1136=EDGE_CURVE('',#899,#901,#544,.T.);
#1137=EDGE_CURVE('',#902,#901,#545,.T.);
#1138=EDGE_CURVE('',#900,#902,#546,.T.);
#1139=EDGE_CURVE('',#901,#895,#547,.T.);
#1140=EDGE_CURVE('',#902,#898,#548,.T.);
#1141=EDGE_CURVE('',#903,#904,#549,.T.);
#1142=EDGE_CURVE('',#905,#904,#550,.T.);
#1143=EDGE_CURVE('',#906,#905,#551,.T.);
#1144=EDGE_CURVE('',#906,#903,#552,.T.);
#1145=EDGE_CURVE('',#904,#907,#553,.T.);
#1146=EDGE_CURVE('',#908,#907,#554,.T.);
#1147=EDGE_CURVE('',#905,#908,#555,.T.);
#1148=EDGE_CURVE('',#907,#909,#556,.T.);
#1149=EDGE_CURVE('',#910,#909,#557,.T.);
#1150=EDGE_CURVE('',#908,#910,#558,.T.);
#1151=EDGE_CURVE('',#909,#903,#559,.T.);
#1152=EDGE_CURVE('',#910,#906,#560,.T.);
#1153=EDGE_CURVE('',#911,#912,#561,.T.);
#1154=EDGE_CURVE('',#913,#912,#562,.T.);
#1155=EDGE_CURVE('',#914,#913,#563,.T.);
#1156=EDGE_CURVE('',#914,#911,#564,.T.);
#1157=EDGE_CURVE('',#912,#915,#565,.T.);
#1158=EDGE_CURVE('',#916,#915,#566,.T.);
#1159=EDGE_CURVE('',#913,#916,#567,.T.);
#1160=EDGE_CURVE('',#915,#917,#568,.T.);
#1161=EDGE_CURVE('',#918,#917,#569,.T.);
#1162=EDGE_CURVE('',#916,#918,#570,.T.);
#1163=EDGE_CURVE('',#917,#919,#571,.T.);
#1164=EDGE_CURVE('',#920,#919,#572,.T.);
#1165=EDGE_CURVE('',#918,#920,#573,.T.);
#1166=EDGE_CURVE('',#919,#911,#574,.T.);
#1167=EDGE_CURVE('',#920,#914,#575,.T.);
#1168=ORIENTED_EDGE('',*,*,#921,.T.);
#1169=ORIENTED_EDGE('',*,*,#922,.T.);
#1170=ORIENTED_EDGE('',*,*,#923,.F.);
#1171=ORIENTED_EDGE('',*,*,#924,.T.);
#1172=ORIENTED_EDGE('',*,*,#925,.T.);
#1173=ORIENTED_EDGE('',*,*,#926,.T.);
#1174=ORIENTED_EDGE('',*,*,#921,.F.);
#1175=ORIENTED_EDGE('',*,*,#927,.T.);
#1176=ORIENTED_EDGE('',*,*,#928,.T.);
#1177=ORIENTED_EDGE('',*,*,#929,.T.);
#1178=ORIENTED_EDGE('',*,*,#925,.F.);
#1179=ORIENTED_EDGE('',*,*,#930,.T.);
#1180=ORIENTED_EDGE('',*,*,#931,.T.);
#1181=ORIENTED_EDGE('',*,*,#932,.T.);
#1182=ORIENTED_EDGE('',*,*,#928,.F.);
#1183=ORIENTED_EDGE('',*,*,#933,.T.);
#1184=ORIENTED_EDGE('',*,*,#934,.T.);
#1185=ORIENTED_EDGE('',*,*,#935,.T.);
#1186=ORIENTED_EDGE('',*,*,#931,.F.);
#1187=ORIENTED_EDGE('',*,*,#936,.T.);
#1188=ORIENTED_EDGE('',*,*,#937,.T.);
#1189=ORIENTED_EDGE('',*,*,#938,.T.);
#1190=ORIENTED_EDGE('',*,*,#934,.F.);
#1191=ORIENTED_EDGE('',*,*,#939,.T.);
#1192=ORIENTED_EDGE('',*,*,#940,.T.);
#1193=ORIENTED_EDGE('',*,*,#941,.T.);
#1194=ORIENTED_EDGE('',*,*,#937,.F.);
#1195=ORIENTED_EDGE('',*,*,#942,.T.);
#1196=ORIENTED_EDGE('',*,*,#923,.T.);
#1197=ORIENTED_EDGE('',*,*,#943,.T.);
#1198=ORIENTED_EDGE('',*,*,#940,.F.);
#1199=ORIENTED_EDGE('',*,*,#944,.T.);
#1200=ORIENTED_EDGE('',*,*,#945,.F.);
#1201=ORIENTED_EDGE('',*,*,#946,.F.);
#1202=ORIENTED_EDGE('',*,*,#947,.F.);
#1203=ORIENTED_EDGE('',*,*,#948,.T.);
#1204=ORIENTED_EDGE('',*,*,#949,.F.);
#1205=ORIENTED_EDGE('',*,*,#948,.F.);
#1206=ORIENTED_EDGE('',*,*,#950,.F.);
#1207=ORIENTED_EDGE('',*,*,#951,.T.);
#1208=ORIENTED_EDGE('',*,*,#952,.F.);
#1209=ORIENTED_EDGE('',*,*,#951,.F.);
#1210=ORIENTED_EDGE('',*,*,#953,.T.);
#1211=ORIENTED_EDGE('',*,*,#954,.T.);
#1212=ORIENTED_EDGE('',*,*,#955,.F.);
#1213=ORIENTED_EDGE('',*,*,#954,.F.);
#1214=ORIENTED_EDGE('',*,*,#956,.F.);
#1215=ORIENTED_EDGE('',*,*,#957,.T.);
#1216=ORIENTED_EDGE('',*,*,#958,.F.);
#1217=ORIENTED_EDGE('',*,*,#957,.F.);
#1218=ORIENTED_EDGE('',*,*,#959,.F.);
#1219=ORIENTED_EDGE('',*,*,#960,.T.);
#1220=ORIENTED_EDGE('',*,*,#961,.F.);
#1221=ORIENTED_EDGE('',*,*,#960,.F.);
#1222=ORIENTED_EDGE('',*,*,#962,.F.);
#1223=ORIENTED_EDGE('',*,*,#963,.T.);
#1224=ORIENTED_EDGE('',*,*,#964,.T.);
#1225=ORIENTED_EDGE('',*,*,#963,.F.);
#1226=ORIENTED_EDGE('',*,*,#965,.F.);
#1227=ORIENTED_EDGE('',*,*,#966,.T.);
#1228=ORIENTED_EDGE('',*,*,#967,.F.);
#1229=ORIENTED_EDGE('',*,*,#966,.F.);
#1230=ORIENTED_EDGE('',*,*,#968,.F.);
#1231=ORIENTED_EDGE('',*,*,#946,.T.);
#1232=ORIENTED_EDGE('',*,*,#962,.T.);
#1233=ORIENTED_EDGE('',*,*,#959,.T.);
#1234=ORIENTED_EDGE('',*,*,#956,.T.);
#1235=ORIENTED_EDGE('',*,*,#953,.F.);
#1236=ORIENTED_EDGE('',*,*,#950,.T.);
#1237=ORIENTED_EDGE('',*,*,#947,.T.);
#1238=ORIENTED_EDGE('',*,*,#968,.T.);
#1239=ORIENTED_EDGE('',*,*,#965,.T.);
#1240=ORIENTED_EDGE('',*,*,#942,.F.);
#1241=ORIENTED_EDGE('',*,*,#939,.F.);
#1242=ORIENTED_EDGE('',*,*,#936,.F.);
#1243=ORIENTED_EDGE('',*,*,#933,.F.);
#1244=ORIENTED_EDGE('',*,*,#930,.F.);
#1245=ORIENTED_EDGE('',*,*,#927,.F.);
#1246=ORIENTED_EDGE('',*,*,#924,.F.);
#1247=ORIENTED_EDGE('',*,*,#944,.F.);
#1248=ORIENTED_EDGE('',*,*,#955,.T.);
#1249=ORIENTED_EDGE('',*,*,#958,.T.);
#1250=ORIENTED_EDGE('',*,*,#961,.T.);
#1251=ORIENTED_EDGE('',*,*,#964,.F.);
#1252=ORIENTED_EDGE('',*,*,#967,.T.);
#1253=ORIENTED_EDGE('',*,*,#945,.T.);
#1254=ORIENTED_EDGE('',*,*,#949,.T.);
#1255=ORIENTED_EDGE('',*,*,#952,.T.);
#1256=ORIENTED_EDGE('',*,*,#926,.F.);
#1257=ORIENTED_EDGE('',*,*,#929,.F.);
#1258=ORIENTED_EDGE('',*,*,#932,.F.);
#1259=ORIENTED_EDGE('',*,*,#935,.F.);
#1260=ORIENTED_EDGE('',*,*,#938,.F.);
#1261=ORIENTED_EDGE('',*,*,#941,.F.);
#1262=ORIENTED_EDGE('',*,*,#943,.F.);
#1263=ORIENTED_EDGE('',*,*,#922,.F.);
#1264=ORIENTED_EDGE('',*,*,#969,.T.);
#1265=ORIENTED_EDGE('',*,*,#970,.T.);
#1266=ORIENTED_EDGE('',*,*,#971,.F.);
#1267=ORIENTED_EDGE('',*,*,#972,.T.);
#1268=ORIENTED_EDGE('',*,*,#973,.T.);
#1269=ORIENTED_EDGE('',*,*,#974,.T.);
#1270=ORIENTED_EDGE('',*,*,#969,.F.);
#1271=ORIENTED_EDGE('',*,*,#975,.T.);
#1272=ORIENTED_EDGE('',*,*,#976,.T.);
#1273=ORIENTED_EDGE('',*,*,#977,.T.);
#1274=ORIENTED_EDGE('',*,*,#973,.F.);
#1275=ORIENTED_EDGE('',*,*,#978,.T.);
#1276=ORIENTED_EDGE('',*,*,#979,.T.);
#1277=ORIENTED_EDGE('',*,*,#980,.T.);
#1278=ORIENTED_EDGE('',*,*,#976,.F.);
#1279=ORIENTED_EDGE('',*,*,#981,.T.);
#1280=ORIENTED_EDGE('',*,*,#982,.T.);
#1281=ORIENTED_EDGE('',*,*,#983,.T.);
#1282=ORIENTED_EDGE('',*,*,#979,.F.);
#1283=ORIENTED_EDGE('',*,*,#984,.T.);
#1284=ORIENTED_EDGE('',*,*,#985,.T.);
#1285=ORIENTED_EDGE('',*,*,#986,.T.);
#1286=ORIENTED_EDGE('',*,*,#982,.F.);
#1287=ORIENTED_EDGE('',*,*,#987,.T.);
#1288=ORIENTED_EDGE('',*,*,#988,.T.);
#1289=ORIENTED_EDGE('',*,*,#989,.T.);
#1290=ORIENTED_EDGE('',*,*,#985,.F.);
#1291=ORIENTED_EDGE('',*,*,#990,.T.);
#1292=ORIENTED_EDGE('',*,*,#971,.T.);
#1293=ORIENTED_EDGE('',*,*,#991,.T.);
#1294=ORIENTED_EDGE('',*,*,#988,.F.);
#1295=ORIENTED_EDGE('',*,*,#992,.T.);
#1296=ORIENTED_EDGE('',*,*,#993,.F.);
#1297=ORIENTED_EDGE('',*,*,#994,.F.);
#1298=ORIENTED_EDGE('',*,*,#995,.F.);
#1299=ORIENTED_EDGE('',*,*,#996,.T.);
#1300=ORIENTED_EDGE('',*,*,#997,.F.);
#1301=ORIENTED_EDGE('',*,*,#996,.F.);
#1302=ORIENTED_EDGE('',*,*,#998,.F.);
#1303=ORIENTED_EDGE('',*,*,#999,.T.);
#1304=ORIENTED_EDGE('',*,*,#1000,.F.);
#1305=ORIENTED_EDGE('',*,*,#999,.F.);
#1306=ORIENTED_EDGE('',*,*,#1001,.T.);
#1307=ORIENTED_EDGE('',*,*,#1002,.T.);
#1308=ORIENTED_EDGE('',*,*,#1003,.F.);
#1309=ORIENTED_EDGE('',*,*,#1002,.F.);
#1310=ORIENTED_EDGE('',*,*,#1004,.F.);
#1311=ORIENTED_EDGE('',*,*,#1005,.T.);
#1312=ORIENTED_EDGE('',*,*,#1006,.F.);
#1313=ORIENTED_EDGE('',*,*,#1005,.F.);
#1314=ORIENTED_EDGE('',*,*,#1007,.F.);
#1315=ORIENTED_EDGE('',*,*,#1008,.T.);
#1316=ORIENTED_EDGE('',*,*,#1009,.F.);
#1317=ORIENTED_EDGE('',*,*,#1008,.F.);
#1318=ORIENTED_EDGE('',*,*,#1010,.F.);
#1319=ORIENTED_EDGE('',*,*,#1011,.T.);
#1320=ORIENTED_EDGE('',*,*,#1012,.T.);
#1321=ORIENTED_EDGE('',*,*,#1011,.F.);
#1322=ORIENTED_EDGE('',*,*,#1013,.F.);
#1323=ORIENTED_EDGE('',*,*,#1014,.T.);
#1324=ORIENTED_EDGE('',*,*,#1015,.F.);
#1325=ORIENTED_EDGE('',*,*,#1014,.F.);
#1326=ORIENTED_EDGE('',*,*,#1016,.F.);
#1327=ORIENTED_EDGE('',*,*,#994,.T.);
#1328=ORIENTED_EDGE('',*,*,#1010,.T.);
#1329=ORIENTED_EDGE('',*,*,#1007,.T.);
#1330=ORIENTED_EDGE('',*,*,#1004,.T.);
#1331=ORIENTED_EDGE('',*,*,#1001,.F.);
#1332=ORIENTED_EDGE('',*,*,#998,.T.);
#1333=ORIENTED_EDGE('',*,*,#995,.T.);
#1334=ORIENTED_EDGE('',*,*,#1016,.T.);
#1335=ORIENTED_EDGE('',*,*,#1013,.T.);
#1336=ORIENTED_EDGE('',*,*,#990,.F.);
#1337=ORIENTED_EDGE('',*,*,#987,.F.);
#1338=ORIENTED_EDGE('',*,*,#984,.F.);
#1339=ORIENTED_EDGE('',*,*,#981,.F.);
#1340=ORIENTED_EDGE('',*,*,#978,.F.);
#1341=ORIENTED_EDGE('',*,*,#975,.F.);
#1342=ORIENTED_EDGE('',*,*,#972,.F.);
#1343=ORIENTED_EDGE('',*,*,#992,.F.);
#1344=ORIENTED_EDGE('',*,*,#1003,.T.);
#1345=ORIENTED_EDGE('',*,*,#1006,.T.);
#1346=ORIENTED_EDGE('',*,*,#1009,.T.);
#1347=ORIENTED_EDGE('',*,*,#1012,.F.);
#1348=ORIENTED_EDGE('',*,*,#1015,.T.);
#1349=ORIENTED_EDGE('',*,*,#993,.T.);
#1350=ORIENTED_EDGE('',*,*,#997,.T.);
#1351=ORIENTED_EDGE('',*,*,#1000,.T.);
#1352=ORIENTED_EDGE('',*,*,#974,.F.);
#1353=ORIENTED_EDGE('',*,*,#977,.F.);
#1354=ORIENTED_EDGE('',*,*,#980,.F.);
#1355=ORIENTED_EDGE('',*,*,#983,.F.);
#1356=ORIENTED_EDGE('',*,*,#986,.F.);
#1357=ORIENTED_EDGE('',*,*,#989,.F.);
#1358=ORIENTED_EDGE('',*,*,#991,.F.);
#1359=ORIENTED_EDGE('',*,*,#970,.F.);
#1360=ORIENTED_EDGE('',*,*,#1017,.F.);
#1361=ORIENTED_EDGE('',*,*,#1018,.T.);
#1362=ORIENTED_EDGE('',*,*,#1019,.T.);
#1363=ORIENTED_EDGE('',*,*,#1020,.F.);
#1364=ORIENTED_EDGE('',*,*,#1021,.F.);
#1365=ORIENTED_EDGE('',*,*,#1020,.T.);
#1366=ORIENTED_EDGE('',*,*,#1022,.T.);
#1367=ORIENTED_EDGE('',*,*,#1023,.F.);
#1368=ORIENTED_EDGE('',*,*,#1024,.F.);
#1369=ORIENTED_EDGE('',*,*,#1023,.T.);
#1370=ORIENTED_EDGE('',*,*,#1025,.T.);
#1371=ORIENTED_EDGE('',*,*,#1026,.F.);
#1372=ORIENTED_EDGE('',*,*,#1027,.F.);
#1373=ORIENTED_EDGE('',*,*,#1026,.T.);
#1374=ORIENTED_EDGE('',*,*,#1028,.T.);
#1375=ORIENTED_EDGE('',*,*,#1029,.F.);
#1376=ORIENTED_EDGE('',*,*,#1030,.F.);
#1377=ORIENTED_EDGE('',*,*,#1029,.T.);
#1378=ORIENTED_EDGE('',*,*,#1031,.T.);
#1379=ORIENTED_EDGE('',*,*,#1032,.F.);
#1380=ORIENTED_EDGE('',*,*,#1033,.F.);
#1381=ORIENTED_EDGE('',*,*,#1032,.T.);
#1382=ORIENTED_EDGE('',*,*,#1034,.T.);
#1383=ORIENTED_EDGE('',*,*,#1035,.F.);
#1384=ORIENTED_EDGE('',*,*,#1036,.F.);
#1385=ORIENTED_EDGE('',*,*,#1035,.T.);
#1386=ORIENTED_EDGE('',*,*,#1037,.T.);
#1387=ORIENTED_EDGE('',*,*,#1038,.F.);
#1388=ORIENTED_EDGE('',*,*,#1039,.F.);
#1389=ORIENTED_EDGE('',*,*,#1040,.T.);
#1390=ORIENTED_EDGE('',*,*,#1041,.T.);
#1391=ORIENTED_EDGE('',*,*,#1042,.F.);
#1392=ORIENTED_EDGE('',*,*,#1043,.F.);
#1393=ORIENTED_EDGE('',*,*,#1044,.T.);
#1394=ORIENTED_EDGE('',*,*,#1039,.T.);
#1395=ORIENTED_EDGE('',*,*,#1045,.F.);
#1396=ORIENTED_EDGE('',*,*,#1046,.F.);
#1397=ORIENTED_EDGE('',*,*,#1047,.T.);
#1398=ORIENTED_EDGE('',*,*,#1043,.T.);
#1399=ORIENTED_EDGE('',*,*,#1048,.F.);
#1400=ORIENTED_EDGE('',*,*,#1049,.F.);
#1401=ORIENTED_EDGE('',*,*,#1050,.T.);
#1402=ORIENTED_EDGE('',*,*,#1046,.T.);
#1403=ORIENTED_EDGE('',*,*,#1051,.F.);
#1404=ORIENTED_EDGE('',*,*,#1052,.F.);
#1405=ORIENTED_EDGE('',*,*,#1053,.T.);
#1406=ORIENTED_EDGE('',*,*,#1049,.T.);
#1407=ORIENTED_EDGE('',*,*,#1054,.F.);
#1408=ORIENTED_EDGE('',*,*,#1055,.F.);
#1409=ORIENTED_EDGE('',*,*,#1056,.T.);
#1410=ORIENTED_EDGE('',*,*,#1052,.T.);
#1411=ORIENTED_EDGE('',*,*,#1057,.F.);
#1412=ORIENTED_EDGE('',*,*,#1058,.F.);
#1413=ORIENTED_EDGE('',*,*,#1059,.T.);
#1414=ORIENTED_EDGE('',*,*,#1055,.T.);
#1415=ORIENTED_EDGE('',*,*,#1060,.F.);
#1416=ORIENTED_EDGE('',*,*,#1041,.F.);
#1417=ORIENTED_EDGE('',*,*,#1061,.T.);
#1418=ORIENTED_EDGE('',*,*,#1058,.T.);
#1419=ORIENTED_EDGE('',*,*,#1062,.F.);
#1420=ORIENTED_EDGE('',*,*,#1063,.F.);
#1421=ORIENTED_EDGE('',*,*,#1038,.T.);
#1422=ORIENTED_EDGE('',*,*,#1064,.T.);
#1423=ORIENTED_EDGE('',*,*,#1018,.F.);
#1424=ORIENTED_EDGE('',*,*,#1019,.F.);
#1425=ORIENTED_EDGE('',*,*,#1064,.F.);
#1426=ORIENTED_EDGE('',*,*,#1037,.F.);
#1427=ORIENTED_EDGE('',*,*,#1034,.F.);
#1428=ORIENTED_EDGE('',*,*,#1031,.F.);
#1429=ORIENTED_EDGE('',*,*,#1028,.F.);
#1430=ORIENTED_EDGE('',*,*,#1025,.F.);
#1431=ORIENTED_EDGE('',*,*,#1022,.F.);
#1432=ORIENTED_EDGE('',*,*,#1042,.T.);
#1433=ORIENTED_EDGE('',*,*,#1062,.T.);
#1434=ORIENTED_EDGE('',*,*,#1060,.T.);
#1435=ORIENTED_EDGE('',*,*,#1057,.T.);
#1436=ORIENTED_EDGE('',*,*,#1054,.T.);
#1437=ORIENTED_EDGE('',*,*,#1051,.T.);
#1438=ORIENTED_EDGE('',*,*,#1048,.T.);
#1439=ORIENTED_EDGE('',*,*,#1045,.T.);
#1440=ORIENTED_EDGE('',*,*,#1063,.T.);
#1441=ORIENTED_EDGE('',*,*,#1017,.T.);
#1442=ORIENTED_EDGE('',*,*,#1021,.T.);
#1443=ORIENTED_EDGE('',*,*,#1024,.T.);
#1444=ORIENTED_EDGE('',*,*,#1027,.T.);
#1445=ORIENTED_EDGE('',*,*,#1030,.T.);
#1446=ORIENTED_EDGE('',*,*,#1033,.T.);
#1447=ORIENTED_EDGE('',*,*,#1036,.T.);
#1448=ORIENTED_EDGE('',*,*,#1040,.F.);
#1449=ORIENTED_EDGE('',*,*,#1044,.F.);
#1450=ORIENTED_EDGE('',*,*,#1047,.F.);
#1451=ORIENTED_EDGE('',*,*,#1050,.F.);
#1452=ORIENTED_EDGE('',*,*,#1053,.F.);
#1453=ORIENTED_EDGE('',*,*,#1056,.F.);
#1454=ORIENTED_EDGE('',*,*,#1059,.F.);
#1455=ORIENTED_EDGE('',*,*,#1061,.F.);
#1456=ORIENTED_EDGE('',*,*,#1065,.F.);
#1457=ORIENTED_EDGE('',*,*,#1066,.T.);
#1458=ORIENTED_EDGE('',*,*,#1067,.T.);
#1459=ORIENTED_EDGE('',*,*,#1068,.F.);
#1460=ORIENTED_EDGE('',*,*,#1069,.F.);
#1461=ORIENTED_EDGE('',*,*,#1068,.T.);
#1462=ORIENTED_EDGE('',*,*,#1070,.T.);
#1463=ORIENTED_EDGE('',*,*,#1071,.F.);
#1464=ORIENTED_EDGE('',*,*,#1072,.F.);
#1465=ORIENTED_EDGE('',*,*,#1071,.T.);
#1466=ORIENTED_EDGE('',*,*,#1073,.T.);
#1467=ORIENTED_EDGE('',*,*,#1074,.F.);
#1468=ORIENTED_EDGE('',*,*,#1075,.F.);
#1469=ORIENTED_EDGE('',*,*,#1074,.T.);
#1470=ORIENTED_EDGE('',*,*,#1076,.T.);
#1471=ORIENTED_EDGE('',*,*,#1077,.F.);
#1472=ORIENTED_EDGE('',*,*,#1078,.F.);
#1473=ORIENTED_EDGE('',*,*,#1077,.T.);
#1474=ORIENTED_EDGE('',*,*,#1079,.T.);
#1475=ORIENTED_EDGE('',*,*,#1080,.F.);
#1476=ORIENTED_EDGE('',*,*,#1081,.F.);
#1477=ORIENTED_EDGE('',*,*,#1080,.T.);
#1478=ORIENTED_EDGE('',*,*,#1082,.T.);
#1479=ORIENTED_EDGE('',*,*,#1083,.F.);
#1480=ORIENTED_EDGE('',*,*,#1084,.F.);
#1481=ORIENTED_EDGE('',*,*,#1083,.T.);
#1482=ORIENTED_EDGE('',*,*,#1085,.T.);
#1483=ORIENTED_EDGE('',*,*,#1086,.F.);
#1484=ORIENTED_EDGE('',*,*,#1087,.F.);
#1485=ORIENTED_EDGE('',*,*,#1088,.T.);
#1486=ORIENTED_EDGE('',*,*,#1089,.T.);
#1487=ORIENTED_EDGE('',*,*,#1090,.F.);
#1488=ORIENTED_EDGE('',*,*,#1091,.F.);
#1489=ORIENTED_EDGE('',*,*,#1092,.T.);
#1490=ORIENTED_EDGE('',*,*,#1087,.T.);
#1491=ORIENTED_EDGE('',*,*,#1093,.F.);
#1492=ORIENTED_EDGE('',*,*,#1094,.F.);
#1493=ORIENTED_EDGE('',*,*,#1095,.T.);
#1494=ORIENTED_EDGE('',*,*,#1091,.T.);
#1495=ORIENTED_EDGE('',*,*,#1096,.F.);
#1496=ORIENTED_EDGE('',*,*,#1097,.F.);
#1497=ORIENTED_EDGE('',*,*,#1098,.T.);
#1498=ORIENTED_EDGE('',*,*,#1094,.T.);
#1499=ORIENTED_EDGE('',*,*,#1099,.F.);
#1500=ORIENTED_EDGE('',*,*,#1100,.F.);
#1501=ORIENTED_EDGE('',*,*,#1101,.T.);
#1502=ORIENTED_EDGE('',*,*,#1097,.T.);
#1503=ORIENTED_EDGE('',*,*,#1102,.F.);
#1504=ORIENTED_EDGE('',*,*,#1103,.F.);
#1505=ORIENTED_EDGE('',*,*,#1104,.T.);
#1506=ORIENTED_EDGE('',*,*,#1100,.T.);
#1507=ORIENTED_EDGE('',*,*,#1105,.F.);
#1508=ORIENTED_EDGE('',*,*,#1106,.F.);
#1509=ORIENTED_EDGE('',*,*,#1107,.T.);
#1510=ORIENTED_EDGE('',*,*,#1103,.T.);
#1511=ORIENTED_EDGE('',*,*,#1108,.F.);
#1512=ORIENTED_EDGE('',*,*,#1089,.F.);
#1513=ORIENTED_EDGE('',*,*,#1109,.T.);
#1514=ORIENTED_EDGE('',*,*,#1106,.T.);
#1515=ORIENTED_EDGE('',*,*,#1110,.F.);
#1516=ORIENTED_EDGE('',*,*,#1111,.F.);
#1517=ORIENTED_EDGE('',*,*,#1086,.T.);
#1518=ORIENTED_EDGE('',*,*,#1112,.T.);
#1519=ORIENTED_EDGE('',*,*,#1066,.F.);
#1520=ORIENTED_EDGE('',*,*,#1067,.F.);
#1521=ORIENTED_EDGE('',*,*,#1112,.F.);
#1522=ORIENTED_EDGE('',*,*,#1085,.F.);
#1523=ORIENTED_EDGE('',*,*,#1082,.F.);
#1524=ORIENTED_EDGE('',*,*,#1079,.F.);
#1525=ORIENTED_EDGE('',*,*,#1076,.F.);
#1526=ORIENTED_EDGE('',*,*,#1073,.F.);
#1527=ORIENTED_EDGE('',*,*,#1070,.F.);
#1528=ORIENTED_EDGE('',*,*,#1090,.T.);
#1529=ORIENTED_EDGE('',*,*,#1110,.T.);
#1530=ORIENTED_EDGE('',*,*,#1108,.T.);
#1531=ORIENTED_EDGE('',*,*,#1105,.T.);
#1532=ORIENTED_EDGE('',*,*,#1102,.T.);
#1533=ORIENTED_EDGE('',*,*,#1099,.T.);
#1534=ORIENTED_EDGE('',*,*,#1096,.T.);
#1535=ORIENTED_EDGE('',*,*,#1093,.T.);
#1536=ORIENTED_EDGE('',*,*,#1111,.T.);
#1537=ORIENTED_EDGE('',*,*,#1065,.T.);
#1538=ORIENTED_EDGE('',*,*,#1069,.T.);
#1539=ORIENTED_EDGE('',*,*,#1072,.T.);
#1540=ORIENTED_EDGE('',*,*,#1075,.T.);
#1541=ORIENTED_EDGE('',*,*,#1078,.T.);
#1542=ORIENTED_EDGE('',*,*,#1081,.T.);
#1543=ORIENTED_EDGE('',*,*,#1084,.T.);
#1544=ORIENTED_EDGE('',*,*,#1088,.F.);
#1545=ORIENTED_EDGE('',*,*,#1092,.F.);
#1546=ORIENTED_EDGE('',*,*,#1095,.F.);
#1547=ORIENTED_EDGE('',*,*,#1098,.F.);
#1548=ORIENTED_EDGE('',*,*,#1101,.F.);
#1549=ORIENTED_EDGE('',*,*,#1104,.F.);
#1550=ORIENTED_EDGE('',*,*,#1107,.F.);
#1551=ORIENTED_EDGE('',*,*,#1109,.F.);
#1552=ORIENTED_EDGE('',*,*,#1113,.T.);
#1553=ORIENTED_EDGE('',*,*,#1114,.T.);
#1554=ORIENTED_EDGE('',*,*,#1115,.T.);
#1555=ORIENTED_EDGE('',*,*,#1116,.T.);
#1556=ORIENTED_EDGE('',*,*,#1117,.T.);
#1557=ORIENTED_EDGE('',*,*,#1118,.T.);
#1558=ORIENTED_EDGE('',*,*,#1119,.T.);
#1559=ORIENTED_EDGE('',*,*,#1120,.T.);
#1560=ORIENTED_EDGE('',*,*,#1121,.T.);
#1561=ORIENTED_EDGE('',*,*,#1122,.T.);
#1562=ORIENTED_EDGE('',*,*,#1123,.T.);
#1563=ORIENTED_EDGE('',*,*,#1124,.T.);
#1564=ORIENTED_EDGE('',*,*,#1125,.T.);
#1565=ORIENTED_EDGE('',*,*,#1126,.T.);
#1566=ORIENTED_EDGE('',*,*,#1127,.T.);
#1567=ORIENTED_EDGE('',*,*,#1128,.T.);
#1568=ORIENTED_EDGE('',*,*,#1129,.T.);
#1569=ORIENTED_EDGE('',*,*,#1130,.F.);
#1570=ORIENTED_EDGE('',*,*,#1131,.F.);
#1571=ORIENTED_EDGE('',*,*,#1132,.T.);
#1572=ORIENTED_EDGE('',*,*,#1133,.T.);
#1573=ORIENTED_EDGE('',*,*,#1134,.F.);
#1574=ORIENTED_EDGE('',*,*,#1135,.F.);
#1575=ORIENTED_EDGE('',*,*,#1130,.T.);
#1576=ORIENTED_EDGE('',*,*,#1136,.T.);
#1577=ORIENTED_EDGE('',*,*,#1137,.F.);
#1578=ORIENTED_EDGE('',*,*,#1138,.F.);
#1579=ORIENTED_EDGE('',*,*,#1134,.T.);
#1580=ORIENTED_EDGE('',*,*,#1139,.T.);
#1581=ORIENTED_EDGE('',*,*,#1132,.F.);
#1582=ORIENTED_EDGE('',*,*,#1140,.F.);
#1583=ORIENTED_EDGE('',*,*,#1137,.T.);
#1584=ORIENTED_EDGE('',*,*,#1131,.T.);
#1585=ORIENTED_EDGE('',*,*,#1135,.T.);
#1586=ORIENTED_EDGE('',*,*,#1138,.T.);
#1587=ORIENTED_EDGE('',*,*,#1140,.T.);
#1588=ORIENTED_EDGE('',*,*,#1129,.F.);
#1589=ORIENTED_EDGE('',*,*,#1139,.F.);
#1590=ORIENTED_EDGE('',*,*,#1136,.F.);
#1591=ORIENTED_EDGE('',*,*,#1133,.F.);
#1592=ORIENTED_EDGE('',*,*,#1141,.T.);
#1593=ORIENTED_EDGE('',*,*,#1142,.F.);
#1594=ORIENTED_EDGE('',*,*,#1143,.F.);
#1595=ORIENTED_EDGE('',*,*,#1144,.T.);
#1596=ORIENTED_EDGE('',*,*,#1145,.T.);
#1597=ORIENTED_EDGE('',*,*,#1146,.F.);
#1598=ORIENTED_EDGE('',*,*,#1147,.F.);
#1599=ORIENTED_EDGE('',*,*,#1142,.T.);
#1600=ORIENTED_EDGE('',*,*,#1148,.T.);
#1601=ORIENTED_EDGE('',*,*,#1149,.F.);
#1602=ORIENTED_EDGE('',*,*,#1150,.F.);
#1603=ORIENTED_EDGE('',*,*,#1146,.T.);
#1604=ORIENTED_EDGE('',*,*,#1151,.T.);
#1605=ORIENTED_EDGE('',*,*,#1144,.F.);
#1606=ORIENTED_EDGE('',*,*,#1152,.F.);
#1607=ORIENTED_EDGE('',*,*,#1149,.T.);
#1608=ORIENTED_EDGE('',*,*,#1143,.T.);
#1609=ORIENTED_EDGE('',*,*,#1147,.T.);
#1610=ORIENTED_EDGE('',*,*,#1150,.T.);
#1611=ORIENTED_EDGE('',*,*,#1152,.T.);
#1612=ORIENTED_EDGE('',*,*,#1141,.F.);
#1613=ORIENTED_EDGE('',*,*,#1151,.F.);
#1614=ORIENTED_EDGE('',*,*,#1148,.F.);
#1615=ORIENTED_EDGE('',*,*,#1145,.F.);
#1616=ORIENTED_EDGE('',*,*,#1153,.T.);
#1617=ORIENTED_EDGE('',*,*,#1154,.F.);
#1618=ORIENTED_EDGE('',*,*,#1155,.F.);
#1619=ORIENTED_EDGE('',*,*,#1156,.T.);
#1620=ORIENTED_EDGE('',*,*,#1157,.T.);
#1621=ORIENTED_EDGE('',*,*,#1158,.F.);
#1622=ORIENTED_EDGE('',*,*,#1159,.F.);
#1623=ORIENTED_EDGE('',*,*,#1154,.T.);
#1624=ORIENTED_EDGE('',*,*,#1160,.T.);
#1625=ORIENTED_EDGE('',*,*,#1161,.F.);
#1626=ORIENTED_EDGE('',*,*,#1162,.F.);
#1627=ORIENTED_EDGE('',*,*,#1158,.T.);
#1628=ORIENTED_EDGE('',*,*,#1163,.T.);
#1629=ORIENTED_EDGE('',*,*,#1164,.F.);
#1630=ORIENTED_EDGE('',*,*,#1165,.F.);
#1631=ORIENTED_EDGE('',*,*,#1161,.T.);
#1632=ORIENTED_EDGE('',*,*,#1166,.T.);
#1633=ORIENTED_EDGE('',*,*,#1156,.F.);
#1634=ORIENTED_EDGE('',*,*,#1167,.F.);
#1635=ORIENTED_EDGE('',*,*,#1164,.T.);
#1636=ORIENTED_EDGE('',*,*,#1155,.T.);
#1637=ORIENTED_EDGE('',*,*,#1159,.T.);
#1638=ORIENTED_EDGE('',*,*,#1162,.T.);
#1639=ORIENTED_EDGE('',*,*,#1165,.T.);
#1640=ORIENTED_EDGE('',*,*,#1167,.T.);
#1641=ORIENTED_EDGE('',*,*,#1153,.F.);
#1642=ORIENTED_EDGE('',*,*,#1166,.F.);
#1643=ORIENTED_EDGE('',*,*,#1163,.F.);
#1644=ORIENTED_EDGE('',*,*,#1160,.F.);
#1645=ORIENTED_EDGE('',*,*,#1157,.F.);
#1646=PLANE('',#1854);
#1647=PLANE('',#1858);
#1648=PLANE('',#1862);
#1649=PLANE('',#1866);
#1650=PLANE('',#1870);
#1651=PLANE('',#1874);
#1652=PLANE('',#1878);
#1653=PLANE('',#1882);
#1654=PLANE('',#1886);
#1655=PLANE('',#1887);
#1656=PLANE('',#1888);
#1657=PLANE('',#1892);
#1658=PLANE('',#1896);
#1659=PLANE('',#1900);
#1660=PLANE('',#1904);
#1661=PLANE('',#1908);
#1662=PLANE('',#1912);
#1663=PLANE('',#1916);
#1664=PLANE('',#1920);
#1665=PLANE('',#1921);
#1666=PLANE('',#1925);
#1667=PLANE('',#1929);
#1668=PLANE('',#1933);
#1669=PLANE('',#1940);
#1670=PLANE('',#1944);
#1671=PLANE('',#1948);
#1672=PLANE('',#1952);
#1673=PLANE('',#1953);
#1674=PLANE('',#1954);
#1675=PLANE('',#1955);
#1676=PLANE('',#1959);
#1677=PLANE('',#1963);
#1678=PLANE('',#1967);
#1679=PLANE('',#1974);
#1680=PLANE('',#1978);
#1681=PLANE('',#1982);
#1682=PLANE('',#1986);
#1683=PLANE('',#1987);
#1684=PLANE('',#1988);
#1685=PLANE('',#1989);
#1686=PLANE('',#1990);
#1687=PLANE('',#1995);
#1688=PLANE('',#2001);
#1689=PLANE('',#2002);
#1690=PLANE('',#2003);
#1691=PLANE('',#2004);
#1692=PLANE('',#2005);
#1693=PLANE('',#2006);
#1694=PLANE('',#2008);
#1695=PLANE('',#2009);
#1696=PLANE('',#2010);
#1697=PLANE('',#2011);
#1698=PLANE('',#2012);
#1699=PLANE('',#2013);
#1700=PLANE('',#2015);
#1701=PLANE('',#2016);
#1702=PLANE('',#2017);
#1703=PLANE('',#2018);
#1704=PLANE('',#2019);
#1705=PLANE('',#2020);
#1706=PLANE('',#2021);
#1707=ADVANCED_FACE('',(#207),#1646,.T.);
#1708=ADVANCED_FACE('',(#208),#175,.F.);
#1709=ADVANCED_FACE('',(#209),#1647,.T.);
#1710=ADVANCED_FACE('',(#210),#176,.F.);
#1711=ADVANCED_FACE('',(#211),#1648,.T.);
#1712=ADVANCED_FACE('',(#212),#177,.F.);
#1713=ADVANCED_FACE('',(#213),#1649,.T.);
#1714=ADVANCED_FACE('',(#214),#178,.F.);
#1715=ADVANCED_FACE('',(#215),#1650,.F.);
#1716=ADVANCED_FACE('',(#216),#179,.T.);
#1717=ADVANCED_FACE('',(#217),#1651,.F.);
#1718=ADVANCED_FACE('',(#218),#180,.T.);
#1719=ADVANCED_FACE('',(#219),#1652,.F.);
#1720=ADVANCED_FACE('',(#220),#181,.T.);
#1721=ADVANCED_FACE('',(#221),#1653,.F.);
#1722=ADVANCED_FACE('',(#222),#182,.T.);
#1723=ADVANCED_FACE('',(#223,#95),#1654,.T.);
#1724=ADVANCED_FACE('',(#224,#96),#1655,.T.);
#1725=ADVANCED_FACE('',(#225),#1656,.T.);
#1726=ADVANCED_FACE('',(#226),#183,.F.);
#1727=ADVANCED_FACE('',(#227),#1657,.T.);
#1728=ADVANCED_FACE('',(#228),#184,.F.);
#1729=ADVANCED_FACE('',(#229),#1658,.T.);
#1730=ADVANCED_FACE('',(#230),#185,.F.);
#1731=ADVANCED_FACE('',(#231),#1659,.T.);
#1732=ADVANCED_FACE('',(#232),#186,.F.);
#1733=ADVANCED_FACE('',(#233),#1660,.F.);
#1734=ADVANCED_FACE('',(#234),#187,.T.);
#1735=ADVANCED_FACE('',(#235),#1661,.F.);
#1736=ADVANCED_FACE('',(#236),#188,.T.);
#1737=ADVANCED_FACE('',(#237),#1662,.F.);
#1738=ADVANCED_FACE('',(#238),#189,.T.);
#1739=ADVANCED_FACE('',(#239),#1663,.F.);
#1740=ADVANCED_FACE('',(#240),#190,.T.);
#1741=ADVANCED_FACE('',(#241,#97),#1664,.T.);
#1742=ADVANCED_FACE('',(#242,#98),#1665,.T.);
#1743=ADVANCED_FACE('',(#243),#191,.T.);
#1744=ADVANCED_FACE('',(#244),#1666,.F.);
#1745=ADVANCED_FACE('',(#245),#192,.T.);
#1746=ADVANCED_FACE('',(#246),#1667,.F.);
#1747=ADVANCED_FACE('',(#247),#193,.T.);
#1748=ADVANCED_FACE('',(#248),#1668,.F.);
#1749=ADVANCED_FACE('',(#249),#194,.T.);
#1750=ADVANCED_FACE('',(#250),#195,.F.);
#1751=ADVANCED_FACE('',(#251),#1669,.T.);
#1752=ADVANCED_FACE('',(#252),#196,.F.);
#1753=ADVANCED_FACE('',(#253),#1670,.T.);
#1754=ADVANCED_FACE('',(#254),#197,.F.);
#1755=ADVANCED_FACE('',(#255),#1671,.T.);
#1756=ADVANCED_FACE('',(#256),#198,.F.);
#1757=ADVANCED_FACE('',(#257),#1672,.T.);
#1758=ADVANCED_FACE('',(#258),#1673,.F.);
#1759=ADVANCED_FACE('',(#259,#99),#1674,.F.);
#1760=ADVANCED_FACE('',(#260,#100),#1675,.T.);
#1761=ADVANCED_FACE('',(#261),#199,.T.);
#1762=ADVANCED_FACE('',(#262),#1676,.F.);
#1763=ADVANCED_FACE('',(#263),#200,.T.);
#1764=ADVANCED_FACE('',(#264),#1677,.F.);
#1765=ADVANCED_FACE('',(#265),#201,.T.);
#1766=ADVANCED_FACE('',(#266),#1678,.F.);
#1767=ADVANCED_FACE('',(#267),#202,.T.);
#1768=ADVANCED_FACE('',(#268),#203,.F.);
#1769=ADVANCED_FACE('',(#269),#1679,.T.);
#1770=ADVANCED_FACE('',(#270),#204,.F.);
#1771=ADVANCED_FACE('',(#271),#1680,.T.);
#1772=ADVANCED_FACE('',(#272),#205,.F.);
#1773=ADVANCED_FACE('',(#273),#1681,.T.);
#1774=ADVANCED_FACE('',(#274),#206,.F.);
#1775=ADVANCED_FACE('',(#275),#1682,.T.);
#1776=ADVANCED_FACE('',(#276),#1683,.F.);
#1777=ADVANCED_FACE('',(#277,#101),#1684,.F.);
#1778=ADVANCED_FACE('',(#278,#102),#1685,.T.);
#1779=ADVANCED_FACE('',(#279),#1686,.T.);
#1780=ADVANCED_FACE('',(#280),#1687,.T.);
#1781=ADVANCED_FACE('',(#281),#1688,.F.);
#1782=ADVANCED_FACE('',(#282),#1689,.F.);
#1783=ADVANCED_FACE('',(#283),#1690,.F.);
#1784=ADVANCED_FACE('',(#284),#1691,.F.);
#1785=ADVANCED_FACE('',(#285),#1692,.T.);
#1786=ADVANCED_FACE('',(#286),#1693,.F.);
#1787=ADVANCED_FACE('',(#287),#1694,.F.);
#1788=ADVANCED_FACE('',(#288),#1695,.F.);
#1789=ADVANCED_FACE('',(#289),#1696,.F.);
#1790=ADVANCED_FACE('',(#290),#1697,.F.);
#1791=ADVANCED_FACE('',(#291),#1698,.F.);
#1792=ADVANCED_FACE('',(#292),#1699,.T.);
#1793=ADVANCED_FACE('',(#293),#1700,.F.);
#1794=ADVANCED_FACE('',(#294),#1701,.F.);
#1795=ADVANCED_FACE('',(#295),#1702,.F.);
#1796=ADVANCED_FACE('',(#296),#1703,.F.);
#1797=ADVANCED_FACE('',(#297),#1704,.F.);
#1798=ADVANCED_FACE('',(#298),#1705,.F.);
#1799=ADVANCED_FACE('',(#299),#1706,.T.);
#1800=CLOSED_SHELL('',(#1707,#1708,#1709,#1710,#1711,#1712,#1713,#1714,
#1715,#1716,#1717,#1718,#1719,#1720,#1721,#1722,#1723,#1724));
#1801=CLOSED_SHELL('',(#1725,#1726,#1727,#1728,#1729,#1730,#1731,#1732,
#1733,#1734,#1735,#1736,#1737,#1738,#1739,#1740,#1741,#1742));
#1802=CLOSED_SHELL('',(#1743,#1744,#1745,#1746,#1747,#1748,#1749,#1750,
#1751,#1752,#1753,#1754,#1755,#1756,#1757,#1758,#1759,#1760));
#1803=CLOSED_SHELL('',(#1761,#1762,#1763,#1764,#1765,#1766,#1767,#1768,
#1769,#1770,#1771,#1772,#1773,#1774,#1775,#1776,#1777,#1778));
#1804=CLOSED_SHELL('',(#1781,#1782,#1783,#1784,#1785,#1786));
#1805=CLOSED_SHELL('',(#1787,#1788,#1789,#1790,#1791,#1792));
#1806=CLOSED_SHELL('',(#1793,#1794,#1795,#1796,#1797,#1798,#1799));
#1807=DERIVED_UNIT_ELEMENT(#1815,1.);
#1808=DERIVED_UNIT_ELEMENT(#3121,-3.);
#1809=DERIVED_UNIT_ELEMENT(#1815,1.);
#1810=DERIVED_UNIT_ELEMENT(#3121,-3.);
#1811=DERIVED_UNIT_ELEMENT(#1815,1.);
#1812=DERIVED_UNIT_ELEMENT(#3121,-3.);
#1813=DERIVED_UNIT_ELEMENT(#1815,1.);
#1814=DERIVED_UNIT_ELEMENT(#3121,-3.);
#1815=(
MASS_UNIT()
NAMED_UNIT(*)
SI_UNIT(.KILO.,.GRAM.)
);
#1816=DERIVED_UNIT((#1807,#1808));
#1817=DERIVED_UNIT((#1809,#1810));
#1818=DERIVED_UNIT((#1811,#1812));
#1819=DERIVED_UNIT((#1813,#1814));
#1820=MEASURE_REPRESENTATION_ITEM('density measure',
POSITIVE_RATIO_MEASURE(7850.),#1816);
#1821=MEASURE_REPRESENTATION_ITEM('density measure',
POSITIVE_RATIO_MEASURE(7850.),#1817);
#1822=MEASURE_REPRESENTATION_ITEM('density measure',
POSITIVE_RATIO_MEASURE(7850.),#1818);
#1823=MEASURE_REPRESENTATION_ITEM('density measure',
POSITIVE_RATIO_MEASURE(7850.),#1819);
#1824=PROPERTY_DEFINITION_REPRESENTATION(#1844,#1832);
#1825=PROPERTY_DEFINITION_REPRESENTATION(#1845,#1833);
#1826=PROPERTY_DEFINITION_REPRESENTATION(#1846,#1834);
#1827=PROPERTY_DEFINITION_REPRESENTATION(#1847,#1835);
#1828=PROPERTY_DEFINITION_REPRESENTATION(#1848,#1836);
#1829=PROPERTY_DEFINITION_REPRESENTATION(#1849,#1837);
#1830=PROPERTY_DEFINITION_REPRESENTATION(#1850,#1838);
#1831=PROPERTY_DEFINITION_REPRESENTATION(#1851,#1839);
#1832=REPRESENTATION('material name',(#1840),#3115);
#1833=REPRESENTATION('density',(#1820),#3115);
#1834=REPRESENTATION('material name',(#1841),#3116);
#1835=REPRESENTATION('density',(#1821),#3116);
#1836=REPRESENTATION('material name',(#1842),#3117);
#1837=REPRESENTATION('density',(#1822),#3117);
#1838=REPRESENTATION('material name',(#1843),#3118);
#1839=REPRESENTATION('density',(#1823),#3118);
#1840=DESCRIPTIVE_REPRESENTATION_ITEM('Steel','Steel');
#1841=DESCRIPTIVE_REPRESENTATION_ITEM('Steel','Steel');
#1842=DESCRIPTIVE_REPRESENTATION_ITEM('Steel','Steel');
#1843=DESCRIPTIVE_REPRESENTATION_ITEM('Steel','Steel');
#1844=PROPERTY_DEFINITION('material property','material name',#3155);
#1845=PROPERTY_DEFINITION('material property','density of part',#3155);
#1846=PROPERTY_DEFINITION('material property','material name',#3156);
#1847=PROPERTY_DEFINITION('material property','density of part',#3156);
#1848=PROPERTY_DEFINITION('material property','material name',#3157);
#1849=PROPERTY_DEFINITION('material property','density of part',#3157);
#1850=PROPERTY_DEFINITION('material property','material name',#3158);
#1851=PROPERTY_DEFINITION('material property','density of part',#3158);
#1852=AXIS2_PLACEMENT_3D('',#2579,#2036,#2037);
#1853=AXIS2_PLACEMENT_3D('',#2580,#2038,#2039);
#1854=AXIS2_PLACEMENT_3D('',#2581,#2040,#2041);
#1855=AXIS2_PLACEMENT_3D('',#2590,#2046,#2047);
#1856=AXIS2_PLACEMENT_3D('',#2594,#2049,#2050);
#1857=AXIS2_PLACEMENT_3D('',#2595,#2051,#2052);
#1858=AXIS2_PLACEMENT_3D('',#2596,#2053,#2054);
#1859=AXIS2_PLACEMENT_3D('',#2602,#2058,#2059);
#1860=AXIS2_PLACEMENT_3D('',#2606,#2061,#2062);
#1861=AXIS2_PLACEMENT_3D('',#2607,#2063,#2064);
#1862=AXIS2_PLACEMENT_3D('',#2608,#2065,#2066);
#1863=AXIS2_PLACEMENT_3D('',#2614,#2070,#2071);
#1864=AXIS2_PLACEMENT_3D('',#2618,#2073,#2074);
#1865=AXIS2_PLACEMENT_3D('',#2619,#2075,#2076);
#1866=AXIS2_PLACEMENT_3D('',#2620,#2077,#2078);
#1867=AXIS2_PLACEMENT_3D('',#2626,#2082,#2083);
#1868=AXIS2_PLACEMENT_3D('',#2627,#2084,#2085);
#1869=AXIS2_PLACEMENT_3D('',#2628,#2086,#2087);
#1870=AXIS2_PLACEMENT_3D('',#2629,#2088,#2089);
#1871=AXIS2_PLACEMENT_3D('',#2638,#2094,#2095);
#1872=AXIS2_PLACEMENT_3D('',#2640,#2096,#2097);
#1873=AXIS2_PLACEMENT_3D('',#2642,#2098,#2099);
#1874=AXIS2_PLACEMENT_3D('',#2644,#2101,#2102);
#1875=AXIS2_PLACEMENT_3D('',#2650,#2106,#2107);
#1876=AXIS2_PLACEMENT_3D('',#2652,#2108,#2109);
#1877=AXIS2_PLACEMENT_3D('',#2654,#2110,#2111);
#1878=AXIS2_PLACEMENT_3D('',#2656,#2113,#2114);
#1879=AXIS2_PLACEMENT_3D('',#2662,#2118,#2119);
#1880=AXIS2_PLACEMENT_3D('',#2664,#2120,#2121);
#1881=AXIS2_PLACEMENT_3D('',#2666,#2122,#2123);
#1882=AXIS2_PLACEMENT_3D('',#2668,#2125,#2126);
#1883=AXIS2_PLACEMENT_3D('',#2674,#2130,#2131);
#1884=AXIS2_PLACEMENT_3D('',#2675,#2132,#2133);
#1885=AXIS2_PLACEMENT_3D('',#2676,#2134,#2135);
#1886=AXIS2_PLACEMENT_3D('',#2677,#2136,#2137);
#1887=AXIS2_PLACEMENT_3D('',#2678,#2138,#2139);
#1888=AXIS2_PLACEMENT_3D('',#2679,#2140,#2141);
#1889=AXIS2_PLACEMENT_3D('',#2688,#2146,#2147);
#1890=AXIS2_PLACEMENT_3D('',#2692,#2149,#2150);
#1891=AXIS2_PLACEMENT_3D('',#2693,#2151,#2152);
#1892=AXIS2_PLACEMENT_3D('',#2694,#2153,#2154);
#1893=AXIS2_PLACEMENT_3D('',#2700,#2158,#2159);
#1894=AXIS2_PLACEMENT_3D('',#2704,#2161,#2162);
#1895=AXIS2_PLACEMENT_3D('',#2705,#2163,#2164);
#1896=AXIS2_PLACEMENT_3D('',#2706,#2165,#2166);
#1897=AXIS2_PLACEMENT_3D('',#2712,#2170,#2171);
#1898=AXIS2_PLACEMENT_3D('',#2716,#2173,#2174);
#1899=AXIS2_PLACEMENT_3D('',#2717,#2175,#2176);
#1900=AXIS2_PLACEMENT_3D('',#2718,#2177,#2178);
#1901=AXIS2_PLACEMENT_3D('',#2724,#2182,#2183);
#1902=AXIS2_PLACEMENT_3D('',#2725,#2184,#2185);
#1903=AXIS2_PLACEMENT_3D('',#2726,#2186,#2187);
#1904=AXIS2_PLACEMENT_3D('',#2727,#2188,#2189);
#1905=AXIS2_PLACEMENT_3D('',#2736,#2194,#2195);
#1906=AXIS2_PLACEMENT_3D('',#2738,#2196,#2197);
#1907=AXIS2_PLACEMENT_3D('',#2740,#2198,#2199);
#1908=AXIS2_PLACEMENT_3D('',#2742,#2201,#2202);
#1909=AXIS2_PLACEMENT_3D('',#2748,#2206,#2207);
#1910=AXIS2_PLACEMENT_3D('',#2750,#2208,#2209);
#1911=AXIS2_PLACEMENT_3D('',#2752,#2210,#2211);
#1912=AXIS2_PLACEMENT_3D('',#2754,#2213,#2214);
#1913=AXIS2_PLACEMENT_3D('',#2760,#2218,#2219);
#1914=AXIS2_PLACEMENT_3D('',#2762,#2220,#2221);
#1915=AXIS2_PLACEMENT_3D('',#2764,#2222,#2223);
#1916=AXIS2_PLACEMENT_3D('',#2766,#2225,#2226);
#1917=AXIS2_PLACEMENT_3D('',#2772,#2230,#2231);
#1918=AXIS2_PLACEMENT_3D('',#2773,#2232,#2233);
#1919=AXIS2_PLACEMENT_3D('',#2774,#2234,#2235);
#1920=AXIS2_PLACEMENT_3D('',#2775,#2236,#2237);
#1921=AXIS2_PLACEMENT_3D('',#2776,#2238,#2239);
#1922=AXIS2_PLACEMENT_3D('',#2777,#2240,#2241);
#1923=AXIS2_PLACEMENT_3D('',#2780,#2242,#2243);
#1924=AXIS2_PLACEMENT_3D('',#2784,#2245,#2246);
#1925=AXIS2_PLACEMENT_3D('',#2786,#2248,#2249);
#1926=AXIS2_PLACEMENT_3D('',#2792,#2253,#2254);
#1927=AXIS2_PLACEMENT_3D('',#2794,#2255,#2256);
#1928=AXIS2_PLACEMENT_3D('',#2796,#2257,#2258);
#1929=AXIS2_PLACEMENT_3D('',#2798,#2260,#2261);
#1930=AXIS2_PLACEMENT_3D('',#2804,#2265,#2266);
#1931=AXIS2_PLACEMENT_3D('',#2806,#2267,#2268);
#1932=AXIS2_PLACEMENT_3D('',#2808,#2269,#2270);
#1933=AXIS2_PLACEMENT_3D('',#2810,#2272,#2273);
#1934=AXIS2_PLACEMENT_3D('',#2816,#2277,#2278);
#1935=AXIS2_PLACEMENT_3D('',#2818,#2279,#2280);
#1936=AXIS2_PLACEMENT_3D('',#2820,#2281,#2282);
#1937=AXIS2_PLACEMENT_3D('',#2822,#2284,#2285);
#1938=AXIS2_PLACEMENT_3D('',#2827,#2287,#2288);
#1939=AXIS2_PLACEMENT_3D('',#2830,#2290,#2291);
#1940=AXIS2_PLACEMENT_3D('',#2831,#2292,#2293);
#1941=AXIS2_PLACEMENT_3D('',#2837,#2297,#2298);
#1942=AXIS2_PLACEMENT_3D('',#2841,#2300,#2301);
#1943=AXIS2_PLACEMENT_3D('',#2842,#2302,#2303);
#1944=AXIS2_PLACEMENT_3D('',#2843,#2304,#2305);
#1945=AXIS2_PLACEMENT_3D('',#2849,#2309,#2310);
#1946=AXIS2_PLACEMENT_3D('',#2853,#2312,#2313);
#1947=AXIS2_PLACEMENT_3D('',#2854,#2314,#2315);
#1948=AXIS2_PLACEMENT_3D('',#2855,#2316,#2317);
#1949=AXIS2_PLACEMENT_3D('',#2861,#2321,#2322);
#1950=AXIS2_PLACEMENT_3D('',#2865,#2324,#2325);
#1951=AXIS2_PLACEMENT_3D('',#2866,#2326,#2327);
#1952=AXIS2_PLACEMENT_3D('',#2867,#2328,#2329);
#1953=AXIS2_PLACEMENT_3D('',#2870,#2332,#2333);
#1954=AXIS2_PLACEMENT_3D('',#2873,#2336,#2337);
#1955=AXIS2_PLACEMENT_3D('',#2874,#2338,#2339);
#1956=AXIS2_PLACEMENT_3D('',#2875,#2340,#2341);
#1957=AXIS2_PLACEMENT_3D('',#2878,#2342,#2343);
#1958=AXIS2_PLACEMENT_3D('',#2882,#2345,#2346);
#1959=AXIS2_PLACEMENT_3D('',#2884,#2348,#2349);
#1960=AXIS2_PLACEMENT_3D('',#2890,#2353,#2354);
#1961=AXIS2_PLACEMENT_3D('',#2892,#2355,#2356);
#1962=AXIS2_PLACEMENT_3D('',#2894,#2357,#2358);
#1963=AXIS2_PLACEMENT_3D('',#2896,#2360,#2361);
#1964=AXIS2_PLACEMENT_3D('',#2902,#2365,#2366);
#1965=AXIS2_PLACEMENT_3D('',#2904,#2367,#2368);
#1966=AXIS2_PLACEMENT_3D('',#2906,#2369,#2370);
#1967=AXIS2_PLACEMENT_3D('',#2908,#2372,#2373);
#1968=AXIS2_PLACEMENT_3D('',#2914,#2377,#2378);
#1969=AXIS2_PLACEMENT_3D('',#2916,#2379,#2380);
#1970=AXIS2_PLACEMENT_3D('',#2918,#2381,#2382);
#1971=AXIS2_PLACEMENT_3D('',#2920,#2384,#2385);
#1972=AXIS2_PLACEMENT_3D('',#2925,#2387,#2388);
#1973=AXIS2_PLACEMENT_3D('',#2928,#2390,#2391);
#1974=AXIS2_PLACEMENT_3D('',#2929,#2392,#2393);
#1975=AXIS2_PLACEMENT_3D('',#2935,#2397,#2398);
#1976=AXIS2_PLACEMENT_3D('',#2939,#2400,#2401);
#1977=AXIS2_PLACEMENT_3D('',#2940,#2402,#2403);
#1978=AXIS2_PLACEMENT_3D('',#2941,#2404,#2405);
#1979=AXIS2_PLACEMENT_3D('',#2947,#2409,#2410);
#1980=AXIS2_PLACEMENT_3D('',#2951,#2412,#2413);
#1981=AXIS2_PLACEMENT_3D('',#2952,#2414,#2415);
#1982=AXIS2_PLACEMENT_3D('',#2953,#2416,#2417);
#1983=AXIS2_PLACEMENT_3D('',#2959,#2421,#2422);
#1984=AXIS2_PLACEMENT_3D('',#2963,#2424,#2425);
#1985=AXIS2_PLACEMENT_3D('',#2964,#2426,#2427);
#1986=AXIS2_PLACEMENT_3D('',#2965,#2428,#2429);
#1987=AXIS2_PLACEMENT_3D('',#2968,#2432,#2433);
#1988=AXIS2_PLACEMENT_3D('',#2971,#2436,#2437);
#1989=AXIS2_PLACEMENT_3D('',#2972,#2438,#2439);
#1990=AXIS2_PLACEMENT_3D('',#2973,#2440,#2441);
#1991=AXIS2_PLACEMENT_3D('',#2976,#2442,#2443);
#1992=AXIS2_PLACEMENT_3D('',#2980,#2445,#2446);
#1993=AXIS2_PLACEMENT_3D('',#2984,#2448,#2449);
#1994=AXIS2_PLACEMENT_3D('',#2988,#2451,#2452);
#1995=AXIS2_PLACEMENT_3D('',#2990,#2454,#2455);
#1996=AXIS2_PLACEMENT_3D('',#2995,#2457,#2458);
#1997=AXIS2_PLACEMENT_3D('',#2999,#2460,#2461);
#1998=AXIS2_PLACEMENT_3D('',#3003,#2463,#2464);
#1999=AXIS2_PLACEMENT_3D('',#3006,#2466,#2467);
#2000=AXIS2_PLACEMENT_3D('',#3007,#2468,#2469);
#2001=AXIS2_PLACEMENT_3D('',#3008,#2470,#2471);
#2002=AXIS2_PLACEMENT_3D('',#3017,#2476,#2477);
#2003=AXIS2_PLACEMENT_3D('',#3023,#2481,#2482);
#2004=AXIS2_PLACEMENT_3D('',#3029,#2486,#2487);
#2005=AXIS2_PLACEMENT_3D('',#3032,#2490,#2491);
#2006=AXIS2_PLACEMENT_3D('',#3033,#2492,#2493);
#2007=AXIS2_PLACEMENT_3D('',#3034,#2494,#2495);
#2008=AXIS2_PLACEMENT_3D('',#3035,#2496,#2497);
#2009=AXIS2_PLACEMENT_3D('',#3044,#2502,#2503);
#2010=AXIS2_PLACEMENT_3D('',#3050,#2507,#2508);
#2011=AXIS2_PLACEMENT_3D('',#3056,#2512,#2513);
#2012=AXIS2_PLACEMENT_3D('',#3059,#2516,#2517);
#2013=AXIS2_PLACEMENT_3D('',#3060,#2518,#2519);
#2014=AXIS2_PLACEMENT_3D('',#3061,#2520,#2521);
#2015=AXIS2_PLACEMENT_3D('',#3062,#2522,#2523);
#2016=AXIS2_PLACEMENT_3D('',#3071,#2528,#2529);
#2017=AXIS2_PLACEMENT_3D('',#3077,#2533,#2534);
#2018=AXIS2_PLACEMENT_3D('',#3083,#2538,#2539);
#2019=AXIS2_PLACEMENT_3D('',#3089,#2543,#2544);
#2020=AXIS2_PLACEMENT_3D('',#3092,#2547,#2548);
#2021=AXIS2_PLACEMENT_3D('',#3093,#2549,#2550);
#2022=AXIS2_PLACEMENT_3D('',#3094,#2551,#2552);
#2023=AXIS2_PLACEMENT_3D('',#3095,#2553,#2554);
#2024=AXIS2_PLACEMENT_3D('',#3096,#2555,#2556);
#2025=AXIS2_PLACEMENT_3D('',#3097,#2557,#2558);
#2026=AXIS2_PLACEMENT_3D('',#3098,#2559,#2560);
#2027=AXIS2_PLACEMENT_3D('',#3099,#2561,#2562);
#2028=AXIS2_PLACEMENT_3D('',#3100,#2563,#2564);
#2029=AXIS2_PLACEMENT_3D('',#3101,#2565,#2566);
#2030=AXIS2_PLACEMENT_3D('',#3102,#2567,#2568);
#2031=AXIS2_PLACEMENT_3D('',#3103,#2569,#2570);
#2032=AXIS2_PLACEMENT_3D('',#3104,#2571,#2572);
#2033=AXIS2_PLACEMENT_3D('',#3105,#2573,#2574);
#2034=AXIS2_PLACEMENT_3D('',#3106,#2575,#2576);
#2035=AXIS2_PLACEMENT_3D('',#3107,#2577,#2578);
#2036=DIRECTION('axis',(0.,0.,1.));
#2037=DIRECTION('refdir',(1.,0.,0.));
#2038=DIRECTION('axis',(0.,0.,1.));
#2039=DIRECTION('refdir',(1.,0.,0.));
#2040=DIRECTION('center_axis',(1.,0.,0.));
#2041=DIRECTION('ref_axis',(0.,0.,-1.));
#2042=DIRECTION('',(0.,-1.,0.));
#2043=DIRECTION('',(0.,0.,-1.));
#2044=DIRECTION('',(0.,-1.,0.));
#2045=DIRECTION('',(0.,0.,1.));
#2046=DIRECTION('center_axis',(0.,-1.,0.));
#2047=DIRECTION('ref_axis',(0.,0.,-1.));
#2048=DIRECTION('',(0.,-1.,0.));
#2049=DIRECTION('center_axis',(0.,-1.,0.));
#2050=DIRECTION('ref_axis',(0.,0.,-1.));
#2051=DIRECTION('center_axis',(0.,1.,0.));
#2052=DIRECTION('ref_axis',(0.,0.,1.));
#2053=DIRECTION('center_axis',(0.,0.,-1.));
#2054=DIRECTION('ref_axis',(-1.,0.,0.));
#2055=DIRECTION('',(0.,-1.,0.));
#2056=DIRECTION('',(-1.,0.,0.));
#2057=DIRECTION('',(1.,0.,0.));
#2058=DIRECTION('center_axis',(0.,-1.,0.));
#2059=DIRECTION('ref_axis',(0.,0.,-1.));
#2060=DIRECTION('',(0.,-1.,0.));
#2061=DIRECTION('center_axis',(0.,-1.,0.));
#2062=DIRECTION('ref_axis',(0.,0.,-1.));
#2063=DIRECTION('center_axis',(0.,1.,0.));
#2064=DIRECTION('ref_axis',(0.,0.,1.));
#2065=DIRECTION('center_axis',(-1.,0.,0.));
#2066=DIRECTION('ref_axis',(0.,0.,1.));
#2067=DIRECTION('',(0.,-1.,0.));
#2068=DIRECTION('',(0.,0.,1.));
#2069=DIRECTION('',(0.,0.,-1.));
#2070=DIRECTION('center_axis',(0.,-1.,0.));
#2071=DIRECTION('ref_axis',(0.,0.,-1.));
#2072=DIRECTION('',(0.,-1.,0.));
#2073=DIRECTION('center_axis',(0.,-1.,0.));
#2074=DIRECTION('ref_axis',(0.,0.,-1.));
#2075=DIRECTION('center_axis',(0.,1.,0.));
#2076=DIRECTION('ref_axis',(0.,0.,1.));
#2077=DIRECTION('center_axis',(0.,0.,1.));
#2078=DIRECTION('ref_axis',(1.,0.,0.));
#2079=DIRECTION('',(0.,-1.,0.));
#2080=DIRECTION('',(1.,0.,0.));
#2081=DIRECTION('',(-1.,0.,0.));
#2082=DIRECTION('center_axis',(0.,-1.,0.));
#2083=DIRECTION('ref_axis',(0.,0.,-1.));
#2084=DIRECTION('center_axis',(0.,-1.,0.));
#2085=DIRECTION('ref_axis',(0.,0.,-1.));
#2086=DIRECTION('center_axis',(0.,1.,0.));
#2087=DIRECTION('ref_axis',(0.,0.,1.));
#2088=DIRECTION('center_axis',(-1.,0.,0.));
#2089=DIRECTION('ref_axis',(0.,0.,1.));
#2090=DIRECTION('',(0.,0.,1.));
#2091=DIRECTION('',(0.,-1.,0.));
#2092=DIRECTION('',(0.,0.,-1.));
#2093=DIRECTION('',(0.,-1.,0.));
#2094=DIRECTION('center_axis',(0.,-1.,0.));
#2095=DIRECTION('ref_axis',(0.,0.,-1.));
#2096=DIRECTION('center_axis',(0.,-1.,0.));
#2097=DIRECTION('ref_axis',(0.,0.,-1.));
#2098=DIRECTION('center_axis',(0.,1.,0.));
#2099=DIRECTION('ref_axis',(0.,0.,1.));
#2100=DIRECTION('',(0.,-1.,0.));
#2101=DIRECTION('center_axis',(0.,0.,-1.));
#2102=DIRECTION('ref_axis',(-1.,0.,0.));
#2103=DIRECTION('',(-1.,0.,0.));
#2104=DIRECTION('',(-1.,0.,0.));
#2105=DIRECTION('',(0.,-1.,0.));
#2106=DIRECTION('center_axis',(0.,-1.,0.));
#2107=DIRECTION('ref_axis',(0.,0.,-1.));
#2108=DIRECTION('center_axis',(0.,-1.,0.));
#2109=DIRECTION('ref_axis',(0.,0.,-1.));
#2110=DIRECTION('center_axis',(0.,1.,0.));
#2111=DIRECTION('ref_axis',(0.,0.,1.));
#2112=DIRECTION('',(0.,-1.,0.));
#2113=DIRECTION('center_axis',(1.,0.,0.));
#2114=DIRECTION('ref_axis',(0.,0.,-1.));
#2115=DIRECTION('',(0.,0.,-1.));
#2116=DIRECTION('',(0.,0.,1.));
#2117=DIRECTION('',(0.,-1.,0.));
#2118=DIRECTION('center_axis',(0.,-1.,0.));
#2119=DIRECTION('ref_axis',(0.,0.,-1.));
#2120=DIRECTION('center_axis',(0.,-1.,0.));
#2121=DIRECTION('ref_axis',(0.,0.,-1.));
#2122=DIRECTION('center_axis',(0.,1.,0.));
#2123=DIRECTION('ref_axis',(0.,0.,1.));
#2124=DIRECTION('',(0.,-1.,0.));
#2125=DIRECTION('center_axis',(0.,0.,1.));
#2126=DIRECTION('ref_axis',(1.,0.,0.));
#2127=DIRECTION('',(-1.,0.,0.));
#2128=DIRECTION('',(-1.,0.,0.));
#2129=DIRECTION('',(0.,-1.,0.));
#2130=DIRECTION('center_axis',(0.,-1.,0.));
#2131=DIRECTION('ref_axis',(0.,0.,-1.));
#2132=DIRECTION('center_axis',(0.,-1.,0.));
#2133=DIRECTION('ref_axis',(0.,0.,-1.));
#2134=DIRECTION('center_axis',(0.,1.,0.));
#2135=DIRECTION('ref_axis',(0.,0.,1.));
#2136=DIRECTION('center_axis',(0.,1.,0.));
#2137=DIRECTION('ref_axis',(0.,0.,1.));
#2138=DIRECTION('center_axis',(0.,-1.,0.));
#2139=DIRECTION('ref_axis',(0.,0.,-1.));
#2140=DIRECTION('center_axis',(1.,0.,0.));
#2141=DIRECTION('ref_axis',(0.,0.,-1.));
#2142=DIRECTION('',(0.,-1.,0.));
#2143=DIRECTION('',(0.,0.,-1.));
#2144=DIRECTION('',(0.,-1.,0.));
#2145=DIRECTION('',(0.,0.,1.));
#2146=DIRECTION('center_axis',(0.,-1.,0.));
#2147=DIRECTION('ref_axis',(0.,0.,-1.));
#2148=DIRECTION('',(0.,-1.,0.));
#2149=DIRECTION('center_axis',(0.,-1.,0.));
#2150=DIRECTION('ref_axis',(0.,0.,-1.));
#2151=DIRECTION('center_axis',(0.,1.,0.));
#2152=DIRECTION('ref_axis',(0.,0.,1.));
#2153=DIRECTION('center_axis',(0.,0.,-1.));
#2154=DIRECTION('ref_axis',(-1.,0.,0.));
#2155=DIRECTION('',(0.,-1.,0.));
#2156=DIRECTION('',(-1.,0.,0.));
#2157=DIRECTION('',(1.,0.,0.));
#2158=DIRECTION('center_axis',(0.,-1.,0.));
#2159=DIRECTION('ref_axis',(0.,0.,-1.));
#2160=DIRECTION('',(0.,-1.,0.));
#2161=DIRECTION('center_axis',(0.,-1.,0.));
#2162=DIRECTION('ref_axis',(0.,0.,-1.));
#2163=DIRECTION('center_axis',(0.,1.,0.));
#2164=DIRECTION('ref_axis',(0.,0.,1.));
#2165=DIRECTION('center_axis',(-1.,0.,0.));
#2166=DIRECTION('ref_axis',(0.,0.,1.));
#2167=DIRECTION('',(0.,-1.,0.));
#2168=DIRECTION('',(0.,0.,1.));
#2169=DIRECTION('',(0.,0.,-1.));
#2170=DIRECTION('center_axis',(0.,-1.,0.));
#2171=DIRECTION('ref_axis',(0.,0.,-1.));
#2172=DIRECTION('',(0.,-1.,0.));
#2173=DIRECTION('center_axis',(0.,-1.,0.));
#2174=DIRECTION('ref_axis',(0.,0.,-1.));
#2175=DIRECTION('center_axis',(0.,1.,0.));
#2176=DIRECTION('ref_axis',(0.,0.,1.));
#2177=DIRECTION('center_axis',(0.,0.,1.));
#2178=DIRECTION('ref_axis',(1.,0.,0.));
#2179=DIRECTION('',(0.,-1.,0.));
#2180=DIRECTION('',(1.,0.,0.));
#2181=DIRECTION('',(-1.,0.,0.));
#2182=DIRECTION('center_axis',(0.,-1.,0.));
#2183=DIRECTION('ref_axis',(0.,0.,-1.));
#2184=DIRECTION('center_axis',(0.,-1.,0.));
#2185=DIRECTION('ref_axis',(0.,0.,-1.));
#2186=DIRECTION('center_axis',(0.,1.,0.));
#2187=DIRECTION('ref_axis',(0.,0.,1.));
#2188=DIRECTION('center_axis',(-1.,0.,0.));
#2189=DIRECTION('ref_axis',(0.,0.,1.));
#2190=DIRECTION('',(0.,0.,1.));
#2191=DIRECTION('',(0.,-1.,0.));
#2192=DIRECTION('',(0.,0.,-1.));
#2193=DIRECTION('',(0.,-1.,0.));
#2194=DIRECTION('center_axis',(0.,-1.,0.));
#2195=DIRECTION('ref_axis',(0.,0.,-1.));
#2196=DIRECTION('center_axis',(0.,-1.,0.));
#2197=DIRECTION('ref_axis',(0.,0.,-1.));
#2198=DIRECTION('center_axis',(0.,1.,0.));
#2199=DIRECTION('ref_axis',(0.,0.,1.));
#2200=DIRECTION('',(0.,-1.,0.));
#2201=DIRECTION('center_axis',(0.,0.,-1.));
#2202=DIRECTION('ref_axis',(-1.,0.,0.));
#2203=DIRECTION('',(-1.,0.,0.));
#2204=DIRECTION('',(-1.,0.,0.));
#2205=DIRECTION('',(0.,-1.,0.));
#2206=DIRECTION('center_axis',(0.,-1.,0.));
#2207=DIRECTION('ref_axis',(0.,0.,-1.));
#2208=DIRECTION('center_axis',(0.,-1.,0.));
#2209=DIRECTION('ref_axis',(0.,0.,-1.));
#2210=DIRECTION('center_axis',(0.,1.,0.));
#2211=DIRECTION('ref_axis',(0.,0.,1.));
#2212=DIRECTION('',(0.,-1.,0.));
#2213=DIRECTION('center_axis',(1.,0.,0.));
#2214=DIRECTION('ref_axis',(0.,0.,-1.));
#2215=DIRECTION('',(0.,0.,-1.));
#2216=DIRECTION('',(0.,0.,1.));
#2217=DIRECTION('',(0.,-1.,0.));
#2218=DIRECTION('center_axis',(0.,-1.,0.));
#2219=DIRECTION('ref_axis',(0.,0.,-1.));
#2220=DIRECTION('center_axis',(0.,-1.,0.));
#2221=DIRECTION('ref_axis',(0.,0.,-1.));
#2222=DIRECTION('center_axis',(0.,1.,0.));
#2223=DIRECTION('ref_axis',(0.,0.,1.));
#2224=DIRECTION('',(0.,-1.,0.));
#2225=DIRECTION('center_axis',(0.,0.,1.));
#2226=DIRECTION('ref_axis',(1.,0.,0.));
#2227=DIRECTION('',(-1.,0.,0.));
#2228=DIRECTION('',(-1.,0.,0.));
#2229=DIRECTION('',(0.,-1.,0.));
#2230=DIRECTION('center_axis',(0.,-1.,0.));
#2231=DIRECTION('ref_axis',(0.,0.,-1.));
#2232=DIRECTION('center_axis',(0.,-1.,0.));
#2233=DIRECTION('ref_axis',(0.,0.,-1.));
#2234=DIRECTION('center_axis',(0.,1.,0.));
#2235=DIRECTION('ref_axis',(0.,0.,1.));
#2236=DIRECTION('center_axis',(0.,1.,0.));
#2237=DIRECTION('ref_axis',(0.,0.,1.));
#2238=DIRECTION('center_axis',(0.,-1.,0.));
#2239=DIRECTION('ref_axis',(0.,0.,-1.));
#2240=DIRECTION('center_axis',(-1.,0.,1.29165007961917E-51));
#2241=DIRECTION('ref_axis',(1.29165007961917E-51,0.,1.));
#2242=DIRECTION('center_axis',(1.,0.,-1.29165007961917E-51));
#2243=DIRECTION('ref_axis',(-1.29165007961917E-51,0.,-1.));
#2244=DIRECTION('',(-1.,0.,1.29165007961917E-51));
#2245=DIRECTION('center_axis',(1.,0.,-1.29165007961917E-51));
#2246=DIRECTION('ref_axis',(-1.29165007961917E-51,0.,-1.));
#2247=DIRECTION('',(-1.,0.,1.29165007961917E-51));
#2248=DIRECTION('center_axis',(-1.29165007961917E-51,0.,-1.));
#2249=DIRECTION('ref_axis',(-1.,0.,1.29165007961917E-51));
#2250=DIRECTION('',(0.,-1.,0.));
#2251=DIRECTION('',(0.,-1.,0.));
#2252=DIRECTION('',(-1.,0.,1.29165007961917E-51));
#2253=DIRECTION('center_axis',(-1.,0.,1.29165007961917E-51));
#2254=DIRECTION('ref_axis',(1.29165007961917E-51,0.,1.));
#2255=DIRECTION('center_axis',(1.,0.,-1.29165007961917E-51));
#2256=DIRECTION('ref_axis',(-1.29165007961917E-51,0.,-1.));
#2257=DIRECTION('center_axis',(1.,0.,-1.29165007961917E-51));
#2258=DIRECTION('ref_axis',(-1.29165007961917E-51,0.,-1.));
#2259=DIRECTION('',(-1.,0.,1.29165007961917E-51));
#2260=DIRECTION('center_axis',(0.,1.,0.));
#2261=DIRECTION('ref_axis',(-1.29165007961917E-51,0.,1.));
#2262=DIRECTION('',(1.29165007961917E-51,0.,-1.));
#2263=DIRECTION('',(1.29165007961917E-51,0.,-1.));
#2264=DIRECTION('',(-1.,0.,1.29165007961917E-51));
#2265=DIRECTION('center_axis',(-1.,0.,1.29165007961917E-51));
#2266=DIRECTION('ref_axis',(1.29165007961917E-51,0.,1.));
#2267=DIRECTION('center_axis',(1.,0.,-1.29165007961917E-51));
#2268=DIRECTION('ref_axis',(-1.29165007961917E-51,0.,-1.));
#2269=DIRECTION('center_axis',(1.,0.,-1.29165007961917E-51));
#2270=DIRECTION('ref_axis',(-1.29165007961917E-51,0.,-1.));
#2271=DIRECTION('',(-1.,0.,1.29165007961917E-51));
#2272=DIRECTION('center_axis',(1.29165007961917E-51,0.,1.));
#2273=DIRECTION('ref_axis',(1.,0.,-1.29165007961917E-51));
#2274=DIRECTION('',(0.,1.,0.));
#2275=DIRECTION('',(0.,1.,0.));
#2276=DIRECTION('',(-1.,0.,1.29165007961917E-51));
#2277=DIRECTION('center_axis',(-1.,0.,1.29165007961917E-51));
#2278=DIRECTION('ref_axis',(1.29165007961917E-51,0.,1.));
#2279=DIRECTION('center_axis',(1.,0.,-1.29165007961917E-51));
#2280=DIRECTION('ref_axis',(-1.29165007961917E-51,0.,-1.));
#2281=DIRECTION('center_axis',(1.,0.,-1.29165007961917E-51));
#2282=DIRECTION('ref_axis',(-1.29165007961917E-51,0.,-1.));
#2283=DIRECTION('',(-1.,0.,1.29165007961917E-51));
#2284=DIRECTION('center_axis',(-1.,0.,1.29165007961917E-51));
#2285=DIRECTION('ref_axis',(1.29165007961917E-51,0.,1.));
#2286=DIRECTION('',(-1.,0.,1.29165007961917E-51));
#2287=DIRECTION('center_axis',(1.,0.,-1.29165007961917E-51));
#2288=DIRECTION('ref_axis',(-1.29165007961917E-51,0.,-1.));
#2289=DIRECTION('',(-1.,0.,1.29165007961917E-51));
#2290=DIRECTION('center_axis',(1.,0.,-1.29165007961917E-51));
#2291=DIRECTION('ref_axis',(-1.29165007961917E-51,0.,-1.));
#2292=DIRECTION('center_axis',(-1.29165007961917E-51,0.,-1.));
#2293=DIRECTION('ref_axis',(-1.,0.,1.29165007961917E-51));
#2294=DIRECTION('',(-1.,0.,1.29165007961917E-51));
#2295=DIRECTION('',(0.,-1.,0.));
#2296=DIRECTION('',(0.,-1.,0.));
#2297=DIRECTION('center_axis',(-1.,0.,1.29165007961917E-51));
#2298=DIRECTION('ref_axis',(1.29165007961917E-51,0.,1.));
#2299=DIRECTION('',(-1.,0.,1.29165007961917E-51));
#2300=DIRECTION('center_axis',(1.,0.,-1.29165007961917E-51));
#2301=DIRECTION('ref_axis',(-1.29165007961917E-51,0.,-1.));
#2302=DIRECTION('center_axis',(1.,0.,-1.29165007961917E-51));
#2303=DIRECTION('ref_axis',(-1.29165007961917E-51,0.,-1.));
#2304=DIRECTION('center_axis',(0.,-1.,0.));
#2305=DIRECTION('ref_axis',(1.29165007961917E-51,0.,-1.));
#2306=DIRECTION('',(-1.,0.,1.29165007961917E-51));
#2307=DIRECTION('',(-1.29165007961917E-51,0.,1.));
#2308=DIRECTION('',(-1.29165007961917E-51,0.,1.));
#2309=DIRECTION('center_axis',(-1.,0.,1.29165007961917E-51));
#2310=DIRECTION('ref_axis',(1.29165007961917E-51,0.,1.));
#2311=DIRECTION('',(-1.,0.,1.29165007961917E-51));
#2312=DIRECTION('center_axis',(1.,0.,-1.29165007961917E-51));
#2313=DIRECTION('ref_axis',(-1.29165007961917E-51,0.,-1.));
#2314=DIRECTION('center_axis',(1.,0.,-1.29165007961917E-51));
#2315=DIRECTION('ref_axis',(-1.29165007961917E-51,0.,-1.));
#2316=DIRECTION('center_axis',(1.29165007961917E-51,0.,1.));
#2317=DIRECTION('ref_axis',(1.,0.,-1.29165007961917E-51));
#2318=DIRECTION('',(-1.,0.,1.29165007961917E-51));
#2319=DIRECTION('',(0.,1.,0.));
#2320=DIRECTION('',(0.,1.,0.));
#2321=DIRECTION('center_axis',(-1.,0.,1.29165007961917E-51));
#2322=DIRECTION('ref_axis',(1.29165007961917E-51,0.,1.));
#2323=DIRECTION('',(-1.,0.,1.29165007961917E-51));
#2324=DIRECTION('center_axis',(1.,0.,-1.29165007961917E-51));
#2325=DIRECTION('ref_axis',(-1.29165007961917E-51,0.,-1.));
#2326=DIRECTION('center_axis',(1.,0.,-1.29165007961917E-51));
#2327=DIRECTION('ref_axis',(-1.29165007961917E-51,0.,-1.));
#2328=DIRECTION('center_axis',(0.,1.,0.));
#2329=DIRECTION('ref_axis',(-1.29165007961917E-51,0.,1.));
#2330=DIRECTION('',(1.29165007961917E-51,0.,-1.));
#2331=DIRECTION('',(1.29165007961917E-51,0.,-1.));
#2332=DIRECTION('center_axis',(0.,-1.,0.));
#2333=DIRECTION('ref_axis',(1.29165007961917E-51,0.,-1.));
#2334=DIRECTION('',(-1.29165007961917E-51,0.,1.));
#2335=DIRECTION('',(-1.29165007961917E-51,0.,1.));
#2336=DIRECTION('center_axis',(1.,0.,1.29165007961917E-51));
#2337=DIRECTION('ref_axis',(1.29165007961917E-51,0.,-1.));
#2338=DIRECTION('center_axis',(1.,0.,1.29165007961917E-51));
#2339=DIRECTION('ref_axis',(1.29165007961917E-51,0.,-1.));
#2340=DIRECTION('center_axis',(-1.,0.,1.58362419671978E-50));
#2341=DIRECTION('ref_axis',(1.58362419671978E-50,0.,1.));
#2342=DIRECTION('center_axis',(1.,0.,-1.58362419671978E-50));
#2343=DIRECTION('ref_axis',(-1.58362419671978E-50,0.,-1.));
#2344=DIRECTION('',(-1.,0.,1.58362419671978E-50));
#2345=DIRECTION('center_axis',(1.,0.,-1.58362419671978E-50));
#2346=DIRECTION('ref_axis',(-1.58362419671978E-50,0.,-1.));
#2347=DIRECTION('',(-1.,0.,1.58362419671978E-50));
#2348=DIRECTION('center_axis',(-1.58362419671978E-50,0.,-1.));
#2349=DIRECTION('ref_axis',(-1.,0.,1.58362419671978E-50));
#2350=DIRECTION('',(0.,-1.,0.));
#2351=DIRECTION('',(0.,-1.,0.));
#2352=DIRECTION('',(-1.,0.,1.58362419671978E-50));
#2353=DIRECTION('center_axis',(-1.,0.,1.58362419671978E-50));
#2354=DIRECTION('ref_axis',(1.58362419671978E-50,0.,1.));
#2355=DIRECTION('center_axis',(1.,0.,-1.58362419671978E-50));
#2356=DIRECTION('ref_axis',(-1.58362419671978E-50,0.,-1.));
#2357=DIRECTION('center_axis',(1.,0.,-1.58362419671978E-50));
#2358=DIRECTION('ref_axis',(-1.58362419671978E-50,0.,-1.));
#2359=DIRECTION('',(-1.,0.,1.58362419671978E-50));
#2360=DIRECTION('center_axis',(0.,1.,0.));
#2361=DIRECTION('ref_axis',(-1.58362419671978E-50,0.,1.));
#2362=DIRECTION('',(1.58362419671978E-50,0.,-1.));
#2363=DIRECTION('',(1.58362419671978E-50,0.,-1.));
#2364=DIRECTION('',(-1.,0.,1.58362419671978E-50));
#2365=DIRECTION('center_axis',(-1.,0.,1.58362419671978E-50));
#2366=DIRECTION('ref_axis',(1.58362419671978E-50,0.,1.));
#2367=DIRECTION('center_axis',(1.,0.,-1.58362419671978E-50));
#2368=DIRECTION('ref_axis',(-1.58362419671978E-50,0.,-1.));
#2369=DIRECTION('center_axis',(1.,0.,-1.58362419671978E-50));
#2370=DIRECTION('ref_axis',(-1.58362419671978E-50,0.,-1.));
#2371=DIRECTION('',(-1.,0.,1.58362419671978E-50));
#2372=DIRECTION('center_axis',(1.58362419671978E-50,0.,1.));
#2373=DIRECTION('ref_axis',(1.,0.,-1.58362419671978E-50));
#2374=DIRECTION('',(0.,1.,0.));
#2375=DIRECTION('',(0.,1.,0.));
#2376=DIRECTION('',(-1.,0.,1.58362419671978E-50));
#2377=DIRECTION('center_axis',(-1.,0.,1.58362419671978E-50));
#2378=DIRECTION('ref_axis',(1.58362419671978E-50,0.,1.));
#2379=DIRECTION('center_axis',(1.,0.,-1.58362419671978E-50));
#2380=DIRECTION('ref_axis',(-1.58362419671978E-50,0.,-1.));
#2381=DIRECTION('center_axis',(1.,0.,-1.58362419671978E-50));
#2382=DIRECTION('ref_axis',(-1.58362419671978E-50,0.,-1.));
#2383=DIRECTION('',(-1.,0.,1.58362419671978E-50));
#2384=DIRECTION('center_axis',(-1.,0.,1.58362419671978E-50));
#2385=DIRECTION('ref_axis',(1.58362419671978E-50,0.,1.));
#2386=DIRECTION('',(-1.,0.,1.58362419671978E-50));
#2387=DIRECTION('center_axis',(1.,0.,-1.58362419671978E-50));
#2388=DIRECTION('ref_axis',(-1.58362419671978E-50,0.,-1.));
#2389=DIRECTION('',(-1.,0.,1.58362419671978E-50));
#2390=DIRECTION('center_axis',(1.,0.,-1.58362419671978E-50));
#2391=DIRECTION('ref_axis',(-1.58362419671978E-50,0.,-1.));
#2392=DIRECTION('center_axis',(-1.58362419671978E-50,0.,-1.));
#2393=DIRECTION('ref_axis',(-1.,0.,1.58362419671978E-50));
#2394=DIRECTION('',(-1.,0.,1.58362419671978E-50));
#2395=DIRECTION('',(0.,-1.,0.));
#2396=DIRECTION('',(0.,-1.,0.));
#2397=DIRECTION('center_axis',(-1.,0.,1.58362419671978E-50));
#2398=DIRECTION('ref_axis',(1.58362419671978E-50,0.,1.));
#2399=DIRECTION('',(-1.,0.,1.58362419671978E-50));
#2400=DIRECTION('center_axis',(1.,0.,-1.58362419671978E-50));
#2401=DIRECTION('ref_axis',(-1.58362419671978E-50,0.,-1.));
#2402=DIRECTION('center_axis',(1.,0.,-1.58362419671978E-50));
#2403=DIRECTION('ref_axis',(-1.58362419671978E-50,0.,-1.));
#2404=DIRECTION('center_axis',(0.,-1.,0.));
#2405=DIRECTION('ref_axis',(1.58362419671978E-50,0.,-1.));
#2406=DIRECTION('',(-1.,0.,1.58362419671978E-50));
#2407=DIRECTION('',(-1.58362419671978E-50,0.,1.));
#2408=DIRECTION('',(-1.58362419671978E-50,0.,1.));
#2409=DIRECTION('center_axis',(-1.,0.,1.58362419671978E-50));
#2410=DIRECTION('ref_axis',(1.58362419671978E-50,0.,1.));
#2411=DIRECTION('',(-1.,0.,1.58362419671978E-50));
#2412=DIRECTION('center_axis',(1.,0.,-1.58362419671978E-50));
#2413=DIRECTION('ref_axis',(-1.58362419671978E-50,0.,-1.));
#2414=DIRECTION('center_axis',(1.,0.,-1.58362419671978E-50));
#2415=DIRECTION('ref_axis',(-1.58362419671978E-50,0.,-1.));
#2416=DIRECTION('center_axis',(1.58362419671978E-50,0.,1.));
#2417=DIRECTION('ref_axis',(1.,0.,-1.58362419671978E-50));
#2418=DIRECTION('',(-1.,0.,1.58362419671978E-50));
#2419=DIRECTION('',(0.,1.,0.));
#2420=DIRECTION('',(0.,1.,0.));
#2421=DIRECTION('center_axis',(-1.,0.,1.58362419671978E-50));
#2422=DIRECTION('ref_axis',(1.58362419671978E-50,0.,1.));
#2423=DIRECTION('',(-1.,0.,1.58362419671978E-50));
#2424=DIRECTION('center_axis',(1.,0.,-1.58362419671978E-50));
#2425=DIRECTION('ref_axis',(-1.58362419671978E-50,0.,-1.));
#2426=DIRECTION('center_axis',(1.,0.,-1.58362419671978E-50));
#2427=DIRECTION('ref_axis',(-1.58362419671978E-50,0.,-1.));
#2428=DIRECTION('center_axis',(0.,1.,0.));
#2429=DIRECTION('ref_axis',(-1.58362419671978E-50,0.,1.));
#2430=DIRECTION('',(1.58362419671978E-50,0.,-1.));
#2431=DIRECTION('',(1.58362419671978E-50,0.,-1.));
#2432=DIRECTION('center_axis',(0.,-1.,0.));
#2433=DIRECTION('ref_axis',(1.58362419671978E-50,0.,-1.));
#2434=DIRECTION('',(-1.58362419671978E-50,0.,1.));
#2435=DIRECTION('',(-1.58362419671978E-50,0.,1.));
#2436=DIRECTION('center_axis',(1.,0.,1.58362419671978E-50));
#2437=DIRECTION('ref_axis',(1.58362419671978E-50,0.,-1.));
#2438=DIRECTION('center_axis',(1.,0.,1.58362419671978E-50));
#2439=DIRECTION('ref_axis',(1.58362419671978E-50,0.,-1.));
#2440=DIRECTION('center_axis',(1.,0.,0.));
#2441=DIRECTION('ref_axis',(0.,0.,-1.));
#2442=DIRECTION('center_axis',(1.,0.,0.));
#2443=DIRECTION('ref_axis',(0.,0.,-1.));
#2444=DIRECTION('',(0.,1.,0.));
#2445=DIRECTION('center_axis',(1.,0.,0.));
#2446=DIRECTION('ref_axis',(0.,0.,-1.));
#2447=DIRECTION('',(0.,0.,1.));
#2448=DIRECTION('center_axis',(1.,0.,0.));
#2449=DIRECTION('ref_axis',(0.,0.,-1.));
#2450=DIRECTION('',(0.,-1.,0.));
#2451=DIRECTION('center_axis',(1.,0.,0.));
#2452=DIRECTION('ref_axis',(0.,0.,-1.));
#2453=DIRECTION('',(0.,0.,-1.));
#2454=DIRECTION('center_axis',(1.,0.,0.));
#2455=DIRECTION('ref_axis',(0.,0.,-1.));
#2456=DIRECTION('',(0.,-1.,0.));
#2457=DIRECTION('center_axis',(1.,0.,0.));
#2458=DIRECTION('ref_axis',(0.,0.,-1.));
#2459=DIRECTION('',(0.,0.,-1.));
#2460=DIRECTION('center_axis',(1.,0.,0.));
#2461=DIRECTION('ref_axis',(0.,0.,-1.));
#2462=DIRECTION('',(0.,1.,0.));
#2463=DIRECTION('center_axis',(1.,0.,0.));
#2464=DIRECTION('ref_axis',(0.,0.,-1.));
#2465=DIRECTION('',(0.,0.,1.));
#2466=DIRECTION('center_axis',(1.,0.,0.));
#2467=DIRECTION('ref_axis',(0.,0.,-1.));
#2468=DIRECTION('axis',(0.,0.,1.));
#2469=DIRECTION('refdir',(1.,0.,0.));
#2470=DIRECTION('center_axis',(-1.,-1.06752213906265E-16,0.));
#2471=DIRECTION('ref_axis',(1.06752213906265E-16,-1.,0.));
#2472=DIRECTION('',(-1.06752213906265E-16,1.,0.));
#2473=DIRECTION('',(0.,0.,-1.));
#2474=DIRECTION('',(-1.06752213906265E-16,1.,0.));
#2475=DIRECTION('',(0.,0.,-1.));
#2476=DIRECTION('center_axis',(0.,-1.,0.));
#2477=DIRECTION('ref_axis',(0.,0.,-1.));
#2478=DIRECTION('',(-1.,0.,0.));
#2479=DIRECTION('',(0.,0.,-1.));
#2480=DIRECTION('',(-1.,0.,0.));
#2481=DIRECTION('center_axis',(1.,1.06752213906265E-16,0.));
#2482=DIRECTION('ref_axis',(-1.06752213906265E-16,1.,0.));
#2483=DIRECTION('',(1.06752213906265E-16,-1.,0.));
#2484=DIRECTION('',(0.,0.,-1.));
#2485=DIRECTION('',(1.06752213906265E-16,-1.,0.));
#2486=DIRECTION('center_axis',(0.,1.,0.));
#2487=DIRECTION('ref_axis',(0.,0.,1.));
#2488=DIRECTION('',(1.,0.,0.));
#2489=DIRECTION('',(1.,0.,0.));
#2490=DIRECTION('center_axis',(0.,0.,1.));
#2491=DIRECTION('ref_axis',(1.,0.,0.));
#2492=DIRECTION('center_axis',(0.,0.,1.));
#2493=DIRECTION('ref_axis',(1.,0.,0.));
#2494=DIRECTION('axis',(0.,0.,1.));
#2495=DIRECTION('refdir',(1.,0.,0.));
#2496=DIRECTION('center_axis',(-1.,0.,0.));
#2497=DIRECTION('ref_axis',(0.,0.,1.));
#2498=DIRECTION('',(0.,1.,0.));
#2499=DIRECTION('',(0.,0.,-1.));
#2500=DIRECTION('',(0.,1.,0.));
#2501=DIRECTION('',(0.,0.,-1.));
#2502=DIRECTION('center_axis',(0.,-1.,0.));
#2503=DIRECTION('ref_axis',(0.,0.,-1.));
#2504=DIRECTION('',(-1.,0.,0.));
#2505=DIRECTION('',(0.,0.,-1.));
#2506=DIRECTION('',(-1.,0.,0.));
#2507=DIRECTION('center_axis',(1.,0.,0.));
#2508=DIRECTION('ref_axis',(0.,0.,-1.));
#2509=DIRECTION('',(0.,-1.,0.));
#2510=DIRECTION('',(0.,0.,-1.));
#2511=DIRECTION('',(0.,-1.,0.));
#2512=DIRECTION('center_axis',(0.,1.,0.));
#2513=DIRECTION('ref_axis',(0.,0.,1.));
#2514=DIRECTION('',(1.,0.,0.));
#2515=DIRECTION('',(1.,0.,0.));
#2516=DIRECTION('center_axis',(0.,0.,-1.));
#2517=DIRECTION('ref_axis',(-1.,0.,0.));
#2518=DIRECTION('center_axis',(0.,0.,-1.));
#2519=DIRECTION('ref_axis',(-1.,0.,0.));
#2520=DIRECTION('axis',(0.,0.,1.));
#2521=DIRECTION('refdir',(1.,0.,0.));
#2522=DIRECTION('center_axis',(0.,1.,0.));
#2523=DIRECTION('ref_axis',(0.,0.,1.));
#2524=DIRECTION('',(1.,0.,0.));
#2525=DIRECTION('',(0.,0.,-1.));
#2526=DIRECTION('',(1.,0.,0.));
#2527=DIRECTION('',(0.,0.,-1.));
#2528=DIRECTION('center_axis',(-1.,2.77555756156289E-16,0.));
#2529=DIRECTION('ref_axis',(-2.77555756156289E-16,-1.,0.));
#2530=DIRECTION('',(2.77555756156289E-16,1.,0.));
#2531=DIRECTION('',(0.,0.,-1.));
#2532=DIRECTION('',(2.77555756156289E-16,1.,0.));
#2533=DIRECTION('center_axis',(-0.923076923076923,-0.384615384615385,0.));
#2534=DIRECTION('ref_axis',(0.384615384615385,-0.923076923076923,0.));
#2535=DIRECTION('',(-0.384615384615385,0.923076923076923,0.));
#2536=DIRECTION('',(0.,0.,-1.));
#2537=DIRECTION('',(-0.384615384615385,0.923076923076923,0.));
#2538=DIRECTION('center_axis',(0.,-1.,0.));
#2539=DIRECTION('ref_axis',(0.,0.,-1.));
#2540=DIRECTION('',(-1.,0.,0.));
#2541=DIRECTION('',(0.,0.,-1.));
#2542=DIRECTION('',(-1.,0.,0.));
#2543=DIRECTION('center_axis',(1.,0.,0.));
#2544=DIRECTION('ref_axis',(0.,0.,-1.));
#2545=DIRECTION('',(0.,-1.,0.));
#2546=DIRECTION('',(0.,-1.,0.));
#2547=DIRECTION('center_axis',(0.,0.,-1.));
#2548=DIRECTION('ref_axis',(-1.,0.,0.));
#2549=DIRECTION('center_axis',(0.,0.,-1.));
#2550=DIRECTION('ref_axis',(-1.,0.,0.));
#2551=DIRECTION('',(5.5163887465173E-33,1.,-2.5449877012713E-16));
#2552=DIRECTION('',(1.,-5.5163887465173E-33,-5.5163887465173E-33));
#2553=DIRECTION('',(-1.,5.5163887465173E-33,0.));
#2554=DIRECTION('',(-5.5163887465173E-33,-1.,0.));
#2555=DIRECTION('',(5.5163887465173E-33,1.,-2.5449877012713E-16));
#2556=DIRECTION('',(-5.55111512312578E-17,2.5449877012713E-16,1.));
#2557=DIRECTION('',(0.,0.,1.));
#2558=DIRECTION('',(1.,0.,0.));
#2559=DIRECTION('',(5.5163887465173E-33,1.,-2.5449877012713E-16));
#2560=DIRECTION('',(1.,-5.5163887465173E-33,-5.5163887465173E-33));
#2561=DIRECTION('',(8.32667268468867E-17,1.,-5.11851271850065E-17));
#2562=DIRECTION('',(-1.,8.32667268468867E-17,-9.86286300523683E-17));
#2563=DIRECTION('',(1.,-7.60958661737274E-33,-6.9565941625082E-18));
#2564=DIRECTION('',(5.8741316177507E-33,1.,-2.49469059008082E-16));
#2565=DIRECTION('',(-8.32667268468867E-17,-1.,-2.13120353147615E-17));
#2566=DIRECTION('',(1.,-8.32667268468867E-17,3.1054364006208E-16));
#2567=DIRECTION('',(4.03703936073889E-16,1.,-2.27363293673855E-16));
#2568=DIRECTION('',(1.,-4.03703936073889E-16,2.33486982377251E-16));
#2569=DIRECTION('',(0.,0.,1.));
#2570=DIRECTION('',(1.,0.,0.));
#2571=DIRECTION('',(1.,-2.22044604925031E-16,7.11163512276149E-16));
#2572=DIRECTION('',(2.22044604925032E-16,1.,-2.49469059008082E-16));
#2573=DIRECTION('',(1.38777878078145E-16,1.,2.13120353147615E-17));
#2574=DIRECTION('',(-1.,1.38777878078145E-16,-3.95339944798207E-16));
#2575=DIRECTION('',(-1.,2.22044604925031E-16,-7.05883584860288E-16));
#2576=DIRECTION('',(-2.22044604925031E-16,-1.,-7.83688208616837E-32));
#2577=DIRECTION('',(-1.38777878078145E-16,-1.,5.11851271850065E-17));
#2578=DIRECTION('',(1.,-1.38777878078145E-16,6.07254954807919E-16));
#2579=CARTESIAN_POINT('',(0.,0.,0.));
#2580=CARTESIAN_POINT('',(0.,0.,0.));
#2581=CARTESIAN_POINT('Origin',(280.,950.,30.));
#2582=CARTESIAN_POINT('',(280.,910.,30.));
#2583=CARTESIAN_POINT('',(280.,40.,30.));
#2584=CARTESIAN_POINT('',(280.,950.,30.));
#2585=CARTESIAN_POINT('',(280.,40.,-30.));
#2586=CARTESIAN_POINT('',(280.,40.,30.));
#2587=CARTESIAN_POINT('',(280.,910.,-30.));
#2588=CARTESIAN_POINT('',(280.,950.,-30.));
#2589=CARTESIAN_POINT('',(280.,910.,30.));
#2590=CARTESIAN_POINT('Origin',(285.,950.,30.));
#2591=CARTESIAN_POINT('',(285.,910.,35.));
#2592=CARTESIAN_POINT('',(285.,40.,35.));
#2593=CARTESIAN_POINT('',(285.,950.,35.));
#2594=CARTESIAN_POINT('Origin',(285.,40.,30.));
#2595=CARTESIAN_POINT('Origin',(285.,910.,30.));
#2596=CARTESIAN_POINT('Origin',(285.,950.,35.));
#2597=CARTESIAN_POINT('',(345.,910.,35.));
#2598=CARTESIAN_POINT('',(345.,40.,35.));
#2599=CARTESIAN_POINT('',(345.,950.,35.));
#2600=CARTESIAN_POINT('',(285.,40.,35.));
#2601=CARTESIAN_POINT('',(285.,910.,35.));
#2602=CARTESIAN_POINT('Origin',(345.,950.,30.));
#2603=CARTESIAN_POINT('',(350.,910.,30.));
#2604=CARTESIAN_POINT('',(350.,40.,30.));
#2605=CARTESIAN_POINT('',(350.,950.,30.));
#2606=CARTESIAN_POINT('Origin',(345.,40.,30.));
#2607=CARTESIAN_POINT('Origin',(345.,910.,30.));
#2608=CARTESIAN_POINT('Origin',(350.,950.,-30.));
#2609=CARTESIAN_POINT('',(350.,910.,-30.));
#2610=CARTESIAN_POINT('',(350.,40.,-30.));
#2611=CARTESIAN_POINT('',(350.,950.,-30.));
#2612=CARTESIAN_POINT('',(350.,40.,-30.));
#2613=CARTESIAN_POINT('',(350.,910.,-30.));
#2614=CARTESIAN_POINT('Origin',(345.,950.,-30.));
#2615=CARTESIAN_POINT('',(345.,910.,-35.));
#2616=CARTESIAN_POINT('',(345.,40.,-35.));
#2617=CARTESIAN_POINT('',(345.,950.,-35.));
#2618=CARTESIAN_POINT('Origin',(345.,40.,-30.));
#2619=CARTESIAN_POINT('Origin',(345.,910.,-30.));
#2620=CARTESIAN_POINT('Origin',(345.,950.,-35.));
#2621=CARTESIAN_POINT('',(285.,910.,-35.));
#2622=CARTESIAN_POINT('',(285.,40.0000000000003,-35.));
#2623=CARTESIAN_POINT('',(285.,950.,-35.));
#2624=CARTESIAN_POINT('',(345.,40.,-35.));
#2625=CARTESIAN_POINT('',(345.,910.,-35.));
#2626=CARTESIAN_POINT('Origin',(285.,950.,-30.));
#2627=CARTESIAN_POINT('Origin',(285.,40.,-30.));
#2628=CARTESIAN_POINT('Origin',(285.,910.,-30.));
#2629=CARTESIAN_POINT('Origin',(355.,950.,-30.));
#2630=CARTESIAN_POINT('',(355.,40.,-30.));
#2631=CARTESIAN_POINT('',(355.,40.,30.));
#2632=CARTESIAN_POINT('',(355.,40.,-30.));
#2633=CARTESIAN_POINT('',(355.,910.,-30.));
#2634=CARTESIAN_POINT('',(355.,950.,-30.));
#2635=CARTESIAN_POINT('',(355.,910.,30.));
#2636=CARTESIAN_POINT('',(355.,910.,-30.));
#2637=CARTESIAN_POINT('',(355.,950.,30.));
#2638=CARTESIAN_POINT('Origin',(345.,950.,30.));
#2639=CARTESIAN_POINT('',(345.,40.,40.));
#2640=CARTESIAN_POINT('Origin',(345.,40.,30.));
#2641=CARTESIAN_POINT('',(345.,910.,40.));
#2642=CARTESIAN_POINT('Origin',(345.,910.,30.));
#2643=CARTESIAN_POINT('',(345.,950.,40.));
#2644=CARTESIAN_POINT('Origin',(285.,950.,40.));
#2645=CARTESIAN_POINT('',(285.,40.,40.));
#2646=CARTESIAN_POINT('',(315.,40.,40.));
#2647=CARTESIAN_POINT('',(285.,910.,40.));
#2648=CARTESIAN_POINT('',(315.,910.,40.));
#2649=CARTESIAN_POINT('',(285.,950.,40.));
#2650=CARTESIAN_POINT('Origin',(285.,950.,30.));
#2651=CARTESIAN_POINT('',(275.,40.,30.));
#2652=CARTESIAN_POINT('Origin',(285.,40.,30.));
#2653=CARTESIAN_POINT('',(275.,910.,30.));
#2654=CARTESIAN_POINT('Origin',(285.,910.,30.));
#2655=CARTESIAN_POINT('',(275.,950.,30.));
#2656=CARTESIAN_POINT('Origin',(275.,950.,30.));
#2657=CARTESIAN_POINT('',(275.,40.,-30.));
#2658=CARTESIAN_POINT('',(275.,40.,30.));
#2659=CARTESIAN_POINT('',(275.,910.,-30.));
#2660=CARTESIAN_POINT('',(275.,910.,30.));
#2661=CARTESIAN_POINT('',(275.,950.,-30.));
#2662=CARTESIAN_POINT('Origin',(285.,950.,-30.));
#2663=CARTESIAN_POINT('',(285.,40.,-40.));
#2664=CARTESIAN_POINT('Origin',(285.,40.,-30.));
#2665=CARTESIAN_POINT('',(285.,910.,-40.));
#2666=CARTESIAN_POINT('Origin',(285.,910.,-30.));
#2667=CARTESIAN_POINT('',(285.,950.,-40.));
#2668=CARTESIAN_POINT('Origin',(345.,950.,-40.));
#2669=CARTESIAN_POINT('',(345.,40.0000000000003,-40.));
#2670=CARTESIAN_POINT('',(315.,40.,-40.));
#2671=CARTESIAN_POINT('',(345.,910.,-40.));
#2672=CARTESIAN_POINT('',(315.,910.,-40.));
#2673=CARTESIAN_POINT('',(345.,950.,-40.));
#2674=CARTESIAN_POINT('Origin',(345.,950.,-30.));
#2675=CARTESIAN_POINT('Origin',(345.,40.,-30.));
#2676=CARTESIAN_POINT('Origin',(345.,910.,-30.));
#2677=CARTESIAN_POINT('Origin',(315.,910.,-30.));
#2678=CARTESIAN_POINT('Origin',(315.,40.,30.));
#2679=CARTESIAN_POINT('Origin',(440.,950.,30.));
#2680=CARTESIAN_POINT('',(440.,910.,30.));
#2681=CARTESIAN_POINT('',(440.,40.,30.));
#2682=CARTESIAN_POINT('',(440.,950.,30.));
#2683=CARTESIAN_POINT('',(440.,40.,-30.));
#2684=CARTESIAN_POINT('',(440.,40.,30.));
#2685=CARTESIAN_POINT('',(440.,910.,-30.));
#2686=CARTESIAN_POINT('',(440.,950.,-30.));
#2687=CARTESIAN_POINT('',(440.,910.,30.));
#2688=CARTESIAN_POINT('Origin',(445.,950.,30.));
#2689=CARTESIAN_POINT('',(445.,910.,35.));
#2690=CARTESIAN_POINT('',(445.,40.,35.));
#2691=CARTESIAN_POINT('',(445.,950.,35.));
#2692=CARTESIAN_POINT('Origin',(445.,40.,30.));
#2693=CARTESIAN_POINT('Origin',(445.,910.,30.));
#2694=CARTESIAN_POINT('Origin',(445.,950.,35.));
#2695=CARTESIAN_POINT('',(505.,910.,35.));
#2696=CARTESIAN_POINT('',(505.,40.,35.));
#2697=CARTESIAN_POINT('',(505.,950.,35.));
#2698=CARTESIAN_POINT('',(445.,40.,35.));
#2699=CARTESIAN_POINT('',(445.,910.,35.));
#2700=CARTESIAN_POINT('Origin',(505.,950.,30.));
#2701=CARTESIAN_POINT('',(510.,910.,30.));
#2702=CARTESIAN_POINT('',(510.,40.,30.));
#2703=CARTESIAN_POINT('',(510.,950.,30.));
#2704=CARTESIAN_POINT('Origin',(505.,40.,30.));
#2705=CARTESIAN_POINT('Origin',(505.,910.,30.));
#2706=CARTESIAN_POINT('Origin',(510.,950.,-30.));
#2707=CARTESIAN_POINT('',(510.,910.,-30.));
#2708=CARTESIAN_POINT('',(510.,40.,-30.));
#2709=CARTESIAN_POINT('',(510.,950.,-30.));
#2710=CARTESIAN_POINT('',(510.,40.,-30.));
#2711=CARTESIAN_POINT('',(510.,910.,-30.));
#2712=CARTESIAN_POINT('Origin',(505.,950.,-30.));
#2713=CARTESIAN_POINT('',(505.,910.,-35.));
#2714=CARTESIAN_POINT('',(505.,40.,-35.));
#2715=CARTESIAN_POINT('',(505.,950.,-35.));
#2716=CARTESIAN_POINT('Origin',(505.,40.,-30.));
#2717=CARTESIAN_POINT('Origin',(505.,910.,-30.));
#2718=CARTESIAN_POINT('Origin',(505.,950.,-35.));
#2719=CARTESIAN_POINT('',(445.,910.,-35.));
#2720=CARTESIAN_POINT('',(445.,40.0000000000003,-35.));
#2721=CARTESIAN_POINT('',(445.,950.,-35.));
#2722=CARTESIAN_POINT('',(505.,40.,-35.));
#2723=CARTESIAN_POINT('',(505.,910.,-35.));
#2724=CARTESIAN_POINT('Origin',(445.,950.,-30.));
#2725=CARTESIAN_POINT('Origin',(445.,40.,-30.));
#2726=CARTESIAN_POINT('Origin',(445.,910.,-30.));
#2727=CARTESIAN_POINT('Origin',(515.,950.,-30.));
#2728=CARTESIAN_POINT('',(515.,40.,-30.));
#2729=CARTESIAN_POINT('',(515.,40.,30.));
#2730=CARTESIAN_POINT('',(515.,40.,-30.));
#2731=CARTESIAN_POINT('',(515.,910.,-30.));
#2732=CARTESIAN_POINT('',(515.,950.,-30.));
#2733=CARTESIAN_POINT('',(515.,910.,30.));
#2734=CARTESIAN_POINT('',(515.,910.,-30.));
#2735=CARTESIAN_POINT('',(515.,950.,30.));
#2736=CARTESIAN_POINT('Origin',(505.,950.,30.));
#2737=CARTESIAN_POINT('',(505.,40.,40.));
#2738=CARTESIAN_POINT('Origin',(505.,40.,30.));
#2739=CARTESIAN_POINT('',(505.,910.,40.));
#2740=CARTESIAN_POINT('Origin',(505.,910.,30.));
#2741=CARTESIAN_POINT('',(505.,950.,40.));
#2742=CARTESIAN_POINT('Origin',(445.,950.,40.));
#2743=CARTESIAN_POINT('',(445.,40.,40.));
#2744=CARTESIAN_POINT('',(475.,40.,40.));
#2745=CARTESIAN_POINT('',(445.,910.,40.));
#2746=CARTESIAN_POINT('',(475.,910.,40.));
#2747=CARTESIAN_POINT('',(445.,950.,40.));
#2748=CARTESIAN_POINT('Origin',(445.,950.,30.));
#2749=CARTESIAN_POINT('',(435.,40.,30.));
#2750=CARTESIAN_POINT('Origin',(445.,40.,30.));
#2751=CARTESIAN_POINT('',(435.,910.,30.));
#2752=CARTESIAN_POINT('Origin',(445.,910.,30.));
#2753=CARTESIAN_POINT('',(435.,950.,30.));
#2754=CARTESIAN_POINT('Origin',(435.,950.,30.));
#2755=CARTESIAN_POINT('',(435.,40.,-30.));
#2756=CARTESIAN_POINT('',(435.,40.,30.));
#2757=CARTESIAN_POINT('',(435.,910.,-30.));
#2758=CARTESIAN_POINT('',(435.,910.,30.));
#2759=CARTESIAN_POINT('',(435.,950.,-30.));
#2760=CARTESIAN_POINT('Origin',(445.,950.,-30.));
#2761=CARTESIAN_POINT('',(445.,40.,-40.));
#2762=CARTESIAN_POINT('Origin',(445.,40.,-30.));
#2763=CARTESIAN_POINT('',(445.,910.,-40.));
#2764=CARTESIAN_POINT('Origin',(445.,910.,-30.));
#2765=CARTESIAN_POINT('',(445.,950.,-40.));
#2766=CARTESIAN_POINT('Origin',(505.,950.,-40.));
#2767=CARTESIAN_POINT('',(505.,40.0000000000003,-40.));
#2768=CARTESIAN_POINT('',(475.,40.,-40.));
#2769=CARTESIAN_POINT('',(505.,910.,-40.));
#2770=CARTESIAN_POINT('',(475.,910.,-40.));
#2771=CARTESIAN_POINT('',(505.,950.,-40.));
#2772=CARTESIAN_POINT('Origin',(505.,950.,-30.));
#2773=CARTESIAN_POINT('Origin',(505.,40.,-30.));
#2774=CARTESIAN_POINT('Origin',(505.,910.,-30.));
#2775=CARTESIAN_POINT('Origin',(475.,910.,-30.));
#2776=CARTESIAN_POINT('Origin',(475.,40.,30.));
#2777=CARTESIAN_POINT('Origin',(475.,980.,30.));
#2778=CARTESIAN_POINT('',(515.,990.,30.));
#2779=CARTESIAN_POINT('',(515.,980.,40.));
#2780=CARTESIAN_POINT('Origin',(515.,980.,30.));
#2781=CARTESIAN_POINT('',(-475.,990.,30.));
#2782=CARTESIAN_POINT('',(475.,990.,30.));
#2783=CARTESIAN_POINT('',(-475.,980.,40.));
#2784=CARTESIAN_POINT('Origin',(-475.,980.,30.));
#2785=CARTESIAN_POINT('',(475.,980.,40.));
#2786=CARTESIAN_POINT('Origin',(475.,980.,40.));
#2787=CARTESIAN_POINT('',(515.,920.,40.));
#2788=CARTESIAN_POINT('',(515.,980.,40.));
#2789=CARTESIAN_POINT('',(-475.,920.,40.));
#2790=CARTESIAN_POINT('',(-475.,980.,40.));
#2791=CARTESIAN_POINT('',(475.,920.,40.));
#2792=CARTESIAN_POINT('Origin',(475.,920.,30.));
#2793=CARTESIAN_POINT('',(515.,910.,30.));
#2794=CARTESIAN_POINT('Origin',(515.,920.,30.));
#2795=CARTESIAN_POINT('',(-475.,910.,30.));
#2796=CARTESIAN_POINT('Origin',(-475.,920.,30.));
#2797=CARTESIAN_POINT('',(475.,910.,30.));
#2798=CARTESIAN_POINT('Origin',(475.,910.,-30.));
#2799=CARTESIAN_POINT('',(515.,910.,-30.));
#2800=CARTESIAN_POINT('',(515.,910.,-30.));
#2801=CARTESIAN_POINT('',(-475.,910.,-30.));
#2802=CARTESIAN_POINT('',(-475.,910.,-30.));
#2803=CARTESIAN_POINT('',(475.,910.,-30.));
#2804=CARTESIAN_POINT('Origin',(475.,920.,-30.));
#2805=CARTESIAN_POINT('',(515.,920.,-40.));
#2806=CARTESIAN_POINT('Origin',(515.,920.,-30.));
#2807=CARTESIAN_POINT('',(-475.,920.,-40.));
#2808=CARTESIAN_POINT('Origin',(-475.,920.,-30.));
#2809=CARTESIAN_POINT('',(475.,920.,-40.));
#2810=CARTESIAN_POINT('Origin',(475.,920.,-40.));
#2811=CARTESIAN_POINT('',(515.,980.,-40.));
#2812=CARTESIAN_POINT('',(515.,920.,-40.));
#2813=CARTESIAN_POINT('',(-475.,980.,-40.));
#2814=CARTESIAN_POINT('',(-475.,920.,-40.));
#2815=CARTESIAN_POINT('',(475.,980.,-40.));
#2816=CARTESIAN_POINT('Origin',(475.,980.,-30.));
#2817=CARTESIAN_POINT('',(515.,990.,-30.));
#2818=CARTESIAN_POINT('Origin',(515.,980.,-30.));
#2819=CARTESIAN_POINT('',(-475.,990.,-30.));
#2820=CARTESIAN_POINT('Origin',(-475.,980.,-30.));
#2821=CARTESIAN_POINT('',(475.,990.,-30.));
#2822=CARTESIAN_POINT('Origin',(475.,920.,30.));
#2823=CARTESIAN_POINT('',(515.,920.,35.));
#2824=CARTESIAN_POINT('',(-475.,920.,35.));
#2825=CARTESIAN_POINT('',(475.,920.,35.));
#2826=CARTESIAN_POINT('',(515.,915.,30.));
#2827=CARTESIAN_POINT('Origin',(515.,920.,30.));
#2828=CARTESIAN_POINT('',(-475.,915.,30.));
#2829=CARTESIAN_POINT('',(475.,915.,30.));
#2830=CARTESIAN_POINT('Origin',(-475.,920.,30.));
#2831=CARTESIAN_POINT('Origin',(475.,980.,35.));
#2832=CARTESIAN_POINT('',(515.,980.,35.));
#2833=CARTESIAN_POINT('',(-475.,980.,35.));
#2834=CARTESIAN_POINT('',(475.,980.,35.));
#2835=CARTESIAN_POINT('',(515.,980.,35.));
#2836=CARTESIAN_POINT('',(-475.,980.,35.));
#2837=CARTESIAN_POINT('Origin',(475.,980.,30.));
#2838=CARTESIAN_POINT('',(515.,985.,30.));
#2839=CARTESIAN_POINT('',(-475.,985.,30.));
#2840=CARTESIAN_POINT('',(475.,985.,30.));
#2841=CARTESIAN_POINT('Origin',(515.,980.,30.));
#2842=CARTESIAN_POINT('Origin',(-475.,980.,30.));
#2843=CARTESIAN_POINT('Origin',(475.,985.,30.));
#2844=CARTESIAN_POINT('',(515.,985.,-30.));
#2845=CARTESIAN_POINT('',(-475.,985.,-30.));
#2846=CARTESIAN_POINT('',(475.,985.,-30.));
#2847=CARTESIAN_POINT('',(515.,985.,30.));
#2848=CARTESIAN_POINT('',(-475.,985.,30.));
#2849=CARTESIAN_POINT('Origin',(475.,980.,-30.));
#2850=CARTESIAN_POINT('',(515.,980.,-35.));
#2851=CARTESIAN_POINT('',(-475.,980.,-35.));
#2852=CARTESIAN_POINT('',(475.,980.,-35.));
#2853=CARTESIAN_POINT('Origin',(515.,980.,-30.));
#2854=CARTESIAN_POINT('Origin',(-475.,980.,-30.));
#2855=CARTESIAN_POINT('Origin',(475.,920.,-35.));
#2856=CARTESIAN_POINT('',(515.,920.,-35.));
#2857=CARTESIAN_POINT('',(-475.,920.,-35.));
#2858=CARTESIAN_POINT('',(475.,920.,-35.));
#2859=CARTESIAN_POINT('',(515.,920.,-35.));
#2860=CARTESIAN_POINT('',(-475.,920.,-35.));
#2861=CARTESIAN_POINT('Origin',(475.,920.,-30.));
#2862=CARTESIAN_POINT('',(515.,915.,-30.));
#2863=CARTESIAN_POINT('',(-475.,915.,-30.));
#2864=CARTESIAN_POINT('',(475.,915.,-30.));
#2865=CARTESIAN_POINT('Origin',(515.,920.,-30.));
#2866=CARTESIAN_POINT('Origin',(-475.,920.,-30.));
#2867=CARTESIAN_POINT('Origin',(475.,915.,-30.));
#2868=CARTESIAN_POINT('',(515.,915.,-30.));
#2869=CARTESIAN_POINT('',(-475.,915.,-30.));
#2870=CARTESIAN_POINT('Origin',(475.,990.,30.));
#2871=CARTESIAN_POINT('',(515.,990.,30.));
#2872=CARTESIAN_POINT('',(-475.,990.,30.));
#2873=CARTESIAN_POINT('Origin',(-475.,980.,30.));
#2874=CARTESIAN_POINT('Origin',(515.,950.,-40.));
#2875=CARTESIAN_POINT('Origin',(475.,30.,30.));
#2876=CARTESIAN_POINT('',(515.,40.,30.));
#2877=CARTESIAN_POINT('',(515.,30.,40.));
#2878=CARTESIAN_POINT('Origin',(515.,30.,30.));
#2879=CARTESIAN_POINT('',(-475.,40.,30.));
#2880=CARTESIAN_POINT('',(475.,40.,30.));
#2881=CARTESIAN_POINT('',(-475.,30.,40.));
#2882=CARTESIAN_POINT('Origin',(-475.,30.,30.));
#2883=CARTESIAN_POINT('',(475.,30.,40.));
#2884=CARTESIAN_POINT('Origin',(475.,30.,40.));
#2885=CARTESIAN_POINT('',(515.,-30.,40.));
#2886=CARTESIAN_POINT('',(515.,30.,40.));
#2887=CARTESIAN_POINT('',(-475.,-30.,40.));
#2888=CARTESIAN_POINT('',(-475.,30.,40.));
#2889=CARTESIAN_POINT('',(475.,-30.,40.));
#2890=CARTESIAN_POINT('Origin',(475.,-30.,30.));
#2891=CARTESIAN_POINT('',(515.,-40.,30.));
#2892=CARTESIAN_POINT('Origin',(515.,-30.,30.));
#2893=CARTESIAN_POINT('',(-475.,-40.,30.));
#2894=CARTESIAN_POINT('Origin',(-475.,-30.,30.));
#2895=CARTESIAN_POINT('',(475.,-40.,30.));
#2896=CARTESIAN_POINT('Origin',(475.,-40.,-30.));
#2897=CARTESIAN_POINT('',(515.,-40.,-30.));
#2898=CARTESIAN_POINT('',(515.,-40.,-30.));
#2899=CARTESIAN_POINT('',(-475.,-40.,-30.));
#2900=CARTESIAN_POINT('',(-475.,-40.,-30.));
#2901=CARTESIAN_POINT('',(475.,-40.,-30.));
#2902=CARTESIAN_POINT('Origin',(475.,-30.,-30.));
#2903=CARTESIAN_POINT('',(515.,-30.,-40.));
#2904=CARTESIAN_POINT('Origin',(515.,-30.,-30.));
#2905=CARTESIAN_POINT('',(-475.,-30.,-40.));
#2906=CARTESIAN_POINT('Origin',(-475.,-30.,-30.));
#2907=CARTESIAN_POINT('',(475.,-30.,-40.));
#2908=CARTESIAN_POINT('Origin',(475.,-30.,-40.));
#2909=CARTESIAN_POINT('',(515.,30.,-40.));
#2910=CARTESIAN_POINT('',(515.,-30.,-40.));
#2911=CARTESIAN_POINT('',(-475.,30.,-40.));
#2912=CARTESIAN_POINT('',(-475.,-30.,-40.));
#2913=CARTESIAN_POINT('',(475.,30.,-40.));
#2914=CARTESIAN_POINT('Origin',(475.,30.,-30.));
#2915=CARTESIAN_POINT('',(515.,40.,-30.));
#2916=CARTESIAN_POINT('Origin',(515.,30.,-30.));
#2917=CARTESIAN_POINT('',(-475.,40.,-30.));
#2918=CARTESIAN_POINT('Origin',(-475.,30.,-30.));
#2919=CARTESIAN_POINT('',(475.,40.,-30.));
#2920=CARTESIAN_POINT('Origin',(475.,-30.,30.));
#2921=CARTESIAN_POINT('',(515.,-30.,35.));
#2922=CARTESIAN_POINT('',(-475.,-30.,35.));
#2923=CARTESIAN_POINT('',(475.,-30.,35.));
#2924=CARTESIAN_POINT('',(515.,-35.,30.));
#2925=CARTESIAN_POINT('Origin',(515.,-30.,30.));
#2926=CARTESIAN_POINT('',(-475.,-35.,30.));
#2927=CARTESIAN_POINT('',(475.,-35.,30.));
#2928=CARTESIAN_POINT('Origin',(-475.,-30.,30.));
#2929=CARTESIAN_POINT('Origin',(475.,30.,35.));
#2930=CARTESIAN_POINT('',(515.,30.,35.));
#2931=CARTESIAN_POINT('',(-475.,30.,35.));
#2932=CARTESIAN_POINT('',(475.,30.,35.));
#2933=CARTESIAN_POINT('',(515.,30.,35.));
#2934=CARTESIAN_POINT('',(-475.,30.,35.));
#2935=CARTESIAN_POINT('Origin',(475.,30.,30.));
#2936=CARTESIAN_POINT('',(515.,35.,30.));
#2937=CARTESIAN_POINT('',(-475.,35.,30.));
#2938=CARTESIAN_POINT('',(475.,35.,30.));
#2939=CARTESIAN_POINT('Origin',(515.,30.,30.));
#2940=CARTESIAN_POINT('Origin',(-475.,30.,30.));
#2941=CARTESIAN_POINT('Origin',(475.,35.,30.));
#2942=CARTESIAN_POINT('',(515.,35.,-30.));
#2943=CARTESIAN_POINT('',(-475.,35.,-30.));
#2944=CARTESIAN_POINT('',(475.,35.,-30.));
#2945=CARTESIAN_POINT('',(515.,35.,30.));
#2946=CARTESIAN_POINT('',(-475.,35.,30.));
#2947=CARTESIAN_POINT('Origin',(475.,30.,-30.));
#2948=CARTESIAN_POINT('',(515.,30.,-35.));
#2949=CARTESIAN_POINT('',(-475.,30.,-35.));
#2950=CARTESIAN_POINT('',(475.,30.,-35.));
#2951=CARTESIAN_POINT('Origin',(515.,30.,-30.));
#2952=CARTESIAN_POINT('Origin',(-475.,30.,-30.));
#2953=CARTESIAN_POINT('Origin',(475.,-30.,-35.));
#2954=CARTESIAN_POINT('',(515.,-30.,-35.));
#2955=CARTESIAN_POINT('',(-475.,-30.,-35.));
#2956=CARTESIAN_POINT('',(475.,-30.,-35.));
#2957=CARTESIAN_POINT('',(515.,-30.,-35.));
#2958=CARTESIAN_POINT('',(-475.,-30.,-35.));
#2959=CARTESIAN_POINT('Origin',(475.,-30.,-30.));
#2960=CARTESIAN_POINT('',(515.,-35.,-30.));
#2961=CARTESIAN_POINT('',(-475.,-35.,-30.));
#2962=CARTESIAN_POINT('',(475.,-35.,-30.));
#2963=CARTESIAN_POINT('Origin',(515.,-30.,-30.));
#2964=CARTESIAN_POINT('Origin',(-475.,-30.,-30.));
#2965=CARTESIAN_POINT('Origin',(475.,-35.,-30.));
#2966=CARTESIAN_POINT('',(515.,-35.,-30.));
#2967=CARTESIAN_POINT('',(-475.,-35.,-30.));
#2968=CARTESIAN_POINT('Origin',(475.,40.,30.));
#2969=CARTESIAN_POINT('',(515.,40.,30.));
#2970=CARTESIAN_POINT('',(-475.,40.,30.));
#2971=CARTESIAN_POINT('Origin',(-475.,30.,30.));
#2972=CARTESIAN_POINT('Origin',(515.,-4.89858719658941E-15,40.));
#2973=CARTESIAN_POINT('Origin',(515.,920.,-30.));
#2974=CARTESIAN_POINT('',(515.,915.,-30.));
#2975=CARTESIAN_POINT('',(515.,920.,-35.));
#2976=CARTESIAN_POINT('Origin',(515.,920.,-30.));
#2977=CARTESIAN_POINT('',(515.,980.,-35.));
#2978=CARTESIAN_POINT('',(515.,920.,-35.));
#2979=CARTESIAN_POINT('',(515.,985.,-30.));
#2980=CARTESIAN_POINT('Origin',(515.,980.,-30.));
#2981=CARTESIAN_POINT('',(515.,985.,30.));
#2982=CARTESIAN_POINT('',(515.,985.,30.));
#2983=CARTESIAN_POINT('',(515.,980.,35.));
#2984=CARTESIAN_POINT('Origin',(515.,980.,30.));
#2985=CARTESIAN_POINT('',(515.,920.,35.));
#2986=CARTESIAN_POINT('',(515.,980.,35.));
#2987=CARTESIAN_POINT('',(515.,915.,30.));
#2988=CARTESIAN_POINT('Origin',(515.,920.,30.));
#2989=CARTESIAN_POINT('',(515.,915.,-30.));
#2990=CARTESIAN_POINT('Origin',(515.,-30.,30.));
#2991=CARTESIAN_POINT('',(515.,30.,35.));
#2992=CARTESIAN_POINT('',(515.,-30.,35.));
#2993=CARTESIAN_POINT('',(515.,30.,35.));
#2994=CARTESIAN_POINT('',(515.,-35.,30.));
#2995=CARTESIAN_POINT('Origin',(515.,-30.,30.));
#2996=CARTESIAN_POINT('',(515.,-35.,-30.));
#2997=CARTESIAN_POINT('',(515.,-35.,-30.));
#2998=CARTESIAN_POINT('',(515.,-30.,-35.));
#2999=CARTESIAN_POINT('Origin',(515.,-30.,-30.));
#3000=CARTESIAN_POINT('',(515.,30.,-35.));
#3001=CARTESIAN_POINT('',(515.,-30.,-35.));
#3002=CARTESIAN_POINT('',(515.,35.,-30.));
#3003=CARTESIAN_POINT('Origin',(515.,30.,-30.));
#3004=CARTESIAN_POINT('',(515.,35.,30.));
#3005=CARTESIAN_POINT('',(515.,35.,30.));
#3006=CARTESIAN_POINT('Origin',(515.,30.,30.));
#3007=CARTESIAN_POINT('',(0.,0.,0.));
#3008=CARTESIAN_POINT('Origin',(67.5,130.,5.));
#3009=CARTESIAN_POINT('',(67.5,-130.,-5.));
#3010=CARTESIAN_POINT('',(67.5,130.,-5.));
#3011=CARTESIAN_POINT('',(67.5,130.,-5.));
#3012=CARTESIAN_POINT('',(67.5,130.,5.));
#3013=CARTESIAN_POINT('',(67.5,130.,5.));
#3014=CARTESIAN_POINT('',(67.5,-130.,5.));
#3015=CARTESIAN_POINT('',(67.5,130.,5.));
#3016=CARTESIAN_POINT('',(67.5,-130.,5.));
#3017=CARTESIAN_POINT('Origin',(-67.5,130.,5.));
#3018=CARTESIAN_POINT('',(-67.5,130.,-5.));
#3019=CARTESIAN_POINT('',(-67.5,130.,-5.));
#3020=CARTESIAN_POINT('',(-67.5,130.,5.));
#3021=CARTESIAN_POINT('',(-67.5,130.,5.));
#3022=CARTESIAN_POINT('',(-67.5,130.,5.));
#3023=CARTESIAN_POINT('Origin',(-67.5,130.,5.));
#3024=CARTESIAN_POINT('',(-67.5,-130.,-5.));
#3025=CARTESIAN_POINT('',(-67.5,130.,-5.));
#3026=CARTESIAN_POINT('',(-67.5,-130.,5.));
#3027=CARTESIAN_POINT('',(-67.5,-130.,5.));
#3028=CARTESIAN_POINT('',(-67.5,130.,5.));
#3029=CARTESIAN_POINT('Origin',(-67.5,-130.,5.));
#3030=CARTESIAN_POINT('',(-67.5,-130.,-5.));
#3031=CARTESIAN_POINT('',(-67.5,-130.,5.));
#3032=CARTESIAN_POINT('Origin',(0.,0.,5.));
#3033=CARTESIAN_POINT('Origin',(0.,0.,-5.));
#3034=CARTESIAN_POINT('',(0.,0.,0.));
#3035=CARTESIAN_POINT('Origin',(105.,-92.5,5.));
#3036=CARTESIAN_POINT('',(105.,-92.5,-5.));
#3037=CARTESIAN_POINT('',(105.,92.5,-5.));
#3038=CARTESIAN_POINT('',(105.,-92.5,-5.));
#3039=CARTESIAN_POINT('',(105.,92.5,5.));
#3040=CARTESIAN_POINT('',(105.,92.5,5.));
#3041=CARTESIAN_POINT('',(105.,-92.5,5.));
#3042=CARTESIAN_POINT('',(105.,-92.5,5.));
#3043=CARTESIAN_POINT('',(105.,-92.5,5.));
#3044=CARTESIAN_POINT('Origin',(-105.,92.5,5.));
#3045=CARTESIAN_POINT('',(-105.,92.5,-5.));
#3046=CARTESIAN_POINT('',(-105.,92.5,-5.));
#3047=CARTESIAN_POINT('',(-105.,92.5,5.));
#3048=CARTESIAN_POINT('',(-105.,92.5,5.));
#3049=CARTESIAN_POINT('',(-105.,92.5,5.));
#3050=CARTESIAN_POINT('Origin',(-105.,-92.5,5.));
#3051=CARTESIAN_POINT('',(-105.,-92.5,-5.));
#3052=CARTESIAN_POINT('',(-105.,-92.5,-5.));
#3053=CARTESIAN_POINT('',(-105.,-92.5,5.));
#3054=CARTESIAN_POINT('',(-105.,-92.5,5.));
#3055=CARTESIAN_POINT('',(-105.,-92.5,5.));
#3056=CARTESIAN_POINT('Origin',(-105.,-92.5,5.));
#3057=CARTESIAN_POINT('',(-105.,-92.5,-5.));
#3058=CARTESIAN_POINT('',(-105.,-92.5,5.));
#3059=CARTESIAN_POINT('Origin',(0.,0.,5.));
#3060=CARTESIAN_POINT('Origin',(0.,0.,-5.));
#3061=CARTESIAN_POINT('',(0.,0.,0.));
#3062=CARTESIAN_POINT('Origin',(50.,0.,5.));
#3063=CARTESIAN_POINT('',(0.,0.,-5.));
#3064=CARTESIAN_POINT('',(50.,0.,-5.));
#3065=CARTESIAN_POINT('',(50.,0.,-5.));
#3066=CARTESIAN_POINT('',(50.,0.,5.));
#3067=CARTESIAN_POINT('',(50.,0.,5.));
#3068=CARTESIAN_POINT('',(0.,0.,5.));
#3069=CARTESIAN_POINT('',(50.,0.,5.));
#3070=CARTESIAN_POINT('',(0.,0.,5.));
#3071=CARTESIAN_POINT('Origin',(50.,25.,5.));
#3072=CARTESIAN_POINT('',(50.,25.,-5.));
#3073=CARTESIAN_POINT('',(50.,25.,-5.));
#3074=CARTESIAN_POINT('',(50.,25.,5.));
#3075=CARTESIAN_POINT('',(50.,25.,5.));
#3076=CARTESIAN_POINT('',(50.,25.,5.));
#3077=CARTESIAN_POINT('Origin',(25.,85.,5.));
#3078=CARTESIAN_POINT('',(25.,85.,-5.));
#3079=CARTESIAN_POINT('',(25.,85.,-5.));
#3080=CARTESIAN_POINT('',(25.,85.,5.));
#3081=CARTESIAN_POINT('',(25.,85.,5.));
#3082=CARTESIAN_POINT('',(25.,85.,5.));
#3083=CARTESIAN_POINT('Origin',(0.,85.,5.));
#3084=CARTESIAN_POINT('',(0.,85.,-5.));
#3085=CARTESIAN_POINT('',(0.,85.,-5.));
#3086=CARTESIAN_POINT('',(0.,85.,5.));
#3087=CARTESIAN_POINT('',(0.,85.,5.));
#3088=CARTESIAN_POINT('',(0.,85.,5.));
#3089=CARTESIAN_POINT('Origin',(0.,0.,5.));
#3090=CARTESIAN_POINT('',(0.,0.,-5.));
#3091=CARTESIAN_POINT('',(0.,0.,5.));
#3092=CARTESIAN_POINT('Origin',(0.,0.,5.));
#3093=CARTESIAN_POINT('Origin',(0.,0.,-5.));
#3094=CARTESIAN_POINT('',(2.50000000000022,44.9999999999999,885.));
#3095=CARTESIAN_POINT('',(6.24500451351651E-13,-40.0000000000003,5.));
#3096=CARTESIAN_POINT('',(3.01381216319063E-13,-2.08702794096464E-13,479.999999999999));
#3097=CARTESIAN_POINT('',(950.000000000001,0.,0.));
#3098=CARTESIAN_POINT('',(947.500000000001,44.9999999999995,885.));
#3099=CARTESIAN_POINT('',(-39.9999999999994,-3.05311331771918E-13,4.99999999999999));
#3100=CARTESIAN_POINT('',(5.69072422050837E-13,39.9999999999997,4.99999999999998));
#3101=CARTESIAN_POINT('',(40.0000000000006,-3.40005801291454E-13,4.99999999999998));
#3102=CARTESIAN_POINT('',(475.,44.9999999999996,885.));
#3103=CARTESIAN_POINT('',(0.,0.,0.));
#3104=CARTESIAN_POINT('',(950.000000000002,39.9999999999996,5.00000000000032));
#3105=CARTESIAN_POINT('',(910.000000000001,-3.24485446955348E-13,5.00000000000028));
#3106=CARTESIAN_POINT('',(950.000000000002,-40.0000000000004,5.00000000000034));
#3107=CARTESIAN_POINT('',(990.000000000002,-4.19664303308309E-13,5.00000000000035));
#3108=UNCERTAINTY_MEASURE_WITH_UNIT(LENGTH_MEASURE(0.01),#3120,
'DISTANCE_ACCURACY_VALUE',
'Maximum model space distance between geometric entities at asserted c
onnectivities');
#3109=UNCERTAINTY_MEASURE_WITH_UNIT(LENGTH_MEASURE(0.01),#3120,
'DISTANCE_ACCURACY_VALUE',
'Maximum model space distance between geometric entities at asserted c
onnectivities');
#3110=UNCERTAINTY_MEASURE_WITH_UNIT(LENGTH_MEASURE(0.01),#3120,
'DISTANCE_ACCURACY_VALUE',
'Maximum model space distance between geometric entities at asserted c
onnectivities');
#3111=UNCERTAINTY_MEASURE_WITH_UNIT(LENGTH_MEASURE(0.01),#3120,
'DISTANCE_ACCURACY_VALUE',
'Maximum model space distance between geometric entities at asserted c
onnectivities');
#3112=UNCERTAINTY_MEASURE_WITH_UNIT(LENGTH_MEASURE(0.01),#3120,
'DISTANCE_ACCURACY_VALUE',
'Maximum model space distance between geometric entities at asserted c
onnectivities');
#3113=UNCERTAINTY_MEASURE_WITH_UNIT(LENGTH_MEASURE(0.01),#3120,
'DISTANCE_ACCURACY_VALUE',
'Maximum model space distance between geometric entities at asserted c
onnectivities');
#3114=(
GEOMETRIC_REPRESENTATION_CONTEXT(3)
GLOBAL_UNCERTAINTY_ASSIGNED_CONTEXT((#3108))
GLOBAL_UNIT_ASSIGNED_CONTEXT((#3120,#3122,#3123))
REPRESENTATION_CONTEXT('','3D')
);
#3115=(
GEOMETRIC_REPRESENTATION_CONTEXT(3)
GLOBAL_UNCERTAINTY_ASSIGNED_CONTEXT((#3109))
GLOBAL_UNIT_ASSIGNED_CONTEXT((#3120,#3122,#3123))
REPRESENTATION_CONTEXT('','3D')
);
#3116=(
GEOMETRIC_REPRESENTATION_CONTEXT(3)
GLOBAL_UNCERTAINTY_ASSIGNED_CONTEXT((#3110))
GLOBAL_UNIT_ASSIGNED_CONTEXT((#3120,#3122,#3123))
REPRESENTATION_CONTEXT('','3D')
);
#3117=(
GEOMETRIC_REPRESENTATION_CONTEXT(3)
GLOBAL_UNCERTAINTY_ASSIGNED_CONTEXT((#3111))
GLOBAL_UNIT_ASSIGNED_CONTEXT((#3120,#3122,#3123))
REPRESENTATION_CONTEXT('','3D')
);
#3118=(
GEOMETRIC_REPRESENTATION_CONTEXT(3)
GLOBAL_UNCERTAINTY_ASSIGNED_CONTEXT((#3112))
GLOBAL_UNIT_ASSIGNED_CONTEXT((#3120,#3122,#3123))
REPRESENTATION_CONTEXT('','3D')
);
#3119=(
GEOMETRIC_REPRESENTATION_CONTEXT(3)
GLOBAL_UNCERTAINTY_ASSIGNED_CONTEXT((#3113))
GLOBAL_UNIT_ASSIGNED_CONTEXT((#3120,#3122,#3123))
REPRESENTATION_CONTEXT('','3D')
);
#3120=(
LENGTH_UNIT()
NAMED_UNIT(*)
SI_UNIT(.MILLI.,.METRE.)
);
#3121=(
LENGTH_UNIT()
NAMED_UNIT(*)
SI_UNIT($,.METRE.)
);
#3122=(
NAMED_UNIT(*)
PLANE_ANGLE_UNIT()
SI_UNIT($,.RADIAN.)
);
#3123=(
NAMED_UNIT(*)
SI_UNIT($,.STERADIAN.)
SOLID_ANGLE_UNIT()
);
#3124=SHAPE_DEFINITION_REPRESENTATION(#3129,#3148);
#3125=SHAPE_DEFINITION_REPRESENTATION(#3130,#3149);
#3126=SHAPE_DEFINITION_REPRESENTATION(#3131,#3150);
#3127=SHAPE_DEFINITION_REPRESENTATION(#3132,#3151);
#3128=SHAPE_DEFINITION_REPRESENTATION(#3133,#3152);
#3129=PRODUCT_DEFINITION_SHAPE('',$,#3154);
#3130=PRODUCT_DEFINITION_SHAPE('',$,#3155);
#3131=PRODUCT_DEFINITION_SHAPE('',$,#3156);
#3132=PRODUCT_DEFINITION_SHAPE('',$,#3157);
#3133=PRODUCT_DEFINITION_SHAPE('',$,#3158);
#3134=PRODUCT_DEFINITION_SHAPE($,$,#53);
#3135=PRODUCT_DEFINITION_SHAPE($,$,#54);
#3136=PRODUCT_DEFINITION_SHAPE($,$,#55);
#3137=PRODUCT_DEFINITION_SHAPE($,$,#56);
#3138=PRODUCT_DEFINITION_SHAPE($,$,#57);
#3139=PRODUCT_DEFINITION_SHAPE($,$,#58);
#3140=PRODUCT_DEFINITION_SHAPE($,$,#59);
#3141=PRODUCT_DEFINITION_SHAPE($,$,#60);
#3142=PRODUCT_DEFINITION_SHAPE($,$,#61);
#3143=PRODUCT_DEFINITION_SHAPE($,$,#62);
#3144=PRODUCT_DEFINITION_SHAPE($,$,#63);
#3145=PRODUCT_DEFINITION_SHAPE($,$,#64);
#3146=PRODUCT_DEFINITION_SHAPE($,$,#65);
#3147=PRODUCT_DEFINITION_SHAPE($,$,#66);
#3148=SHAPE_REPRESENTATION('',(#1852,#2022,#2023,#2024,#2025,#2026,#2027,
#2028,#2029,#2030,#2031,#2032,#2033,#2034,#2035),#3114);
#3149=SHAPE_REPRESENTATION('',(#1853,#77,#78),#3115);
#3150=SHAPE_REPRESENTATION('',(#2000),#3116);
#3151=SHAPE_REPRESENTATION('',(#2007),#3117);
#3152=SHAPE_REPRESENTATION('',(#2014),#3118);
#3153=PRODUCT_DEFINITION_CONTEXT('part definition',#3170,'design');
#3154=PRODUCT_DEFINITION('PILLER FRAME','TAS-014',#3159,#3153);
#3155=PRODUCT_DEFINITION('Square Tube','Square Tube',#3160,#3153);
#3156=PRODUCT_DEFINITION('Welded Pad','Welded Pad',#3161,#3153);
#3157=PRODUCT_DEFINITION('Base plate','Base Plate',#3162,#3153);
#3158=PRODUCT_DEFINITION('Welded Pad 2','Welded Pad 2',#3163,#3153);
#3159=PRODUCT_DEFINITION_FORMATION('',$,#3172);
#3160=PRODUCT_DEFINITION_FORMATION('',$,#3173);
#3161=PRODUCT_DEFINITION_FORMATION('',$,#3174);
#3162=PRODUCT_DEFINITION_FORMATION('',$,#3175);
#3163=PRODUCT_DEFINITION_FORMATION('',$,#3176);
#3164=PRODUCT_RELATED_PRODUCT_CATEGORY('TAS-014','TAS-014',(#3172));
#3165=PRODUCT_RELATED_PRODUCT_CATEGORY('Square Tube','Square Tube',(#3173));
#3166=PRODUCT_RELATED_PRODUCT_CATEGORY('Welded Pad','Welded Pad',(#3174));
#3167=PRODUCT_RELATED_PRODUCT_CATEGORY('Base Plate','Base Plate',(#3175));
#3168=PRODUCT_RELATED_PRODUCT_CATEGORY('Welded Pad 2','Welded Pad 2',(#3176));
#3169=APPLICATION_PROTOCOL_DEFINITION('international standard',
'automotive_design',2009,#3170);
#3170=APPLICATION_CONTEXT(
'Core Data for Automotive Mechanical Design Process');
#3171=PRODUCT_CONTEXT('part definition',#3170,'mechanical');
#3172=PRODUCT('PILLER FRAME','TAS-014','STEP AP214',(#3171));
#3173=PRODUCT('Square Tube','Square Tube',$,(#3171));
#3174=PRODUCT('Welded Pad','Welded Pad',$,(#3171));
#3175=PRODUCT('Base plate','Base Plate','Base plate',(#3171));
#3176=PRODUCT('Welded Pad 2','Welded Pad 2',$,(#3171));
#3177=PRESENTATION_STYLE_ASSIGNMENT((#3179));
#3178=PRESENTATION_STYLE_ASSIGNMENT((#3180));
#3179=SURFACE_STYLE_USAGE(.BOTH.,#3181);
#3180=SURFACE_STYLE_USAGE(.BOTH.,#3182);
#3181=SURFACE_SIDE_STYLE('',(#3183));
#3182=SURFACE_SIDE_STYLE('',(#3184));
#3183=SURFACE_STYLE_FILL_AREA(#3185);
#3184=SURFACE_STYLE_FILL_AREA(#3186);
#3185=FILL_AREA_STYLE('Steel - Satin',(#3187));
#3186=FILL_AREA_STYLE('Opaque(202,209,238)',(#3188));
#3187=FILL_AREA_STYLE_COLOUR('Steel - Satin',#3189);
#3188=FILL_AREA_STYLE_COLOUR('Opaque(202,209,238)',#3190);
#3189=COLOUR_RGB('Steel - Satin',0.627450980392157,0.627450980392157,0.627450980392157);
#3190=COLOUR_RGB('Opaque(202,209,238)',0.792156862745098,0.819607843137255,
0.933333333333333);
ENDSEC;
END-ISO-10303-21;
